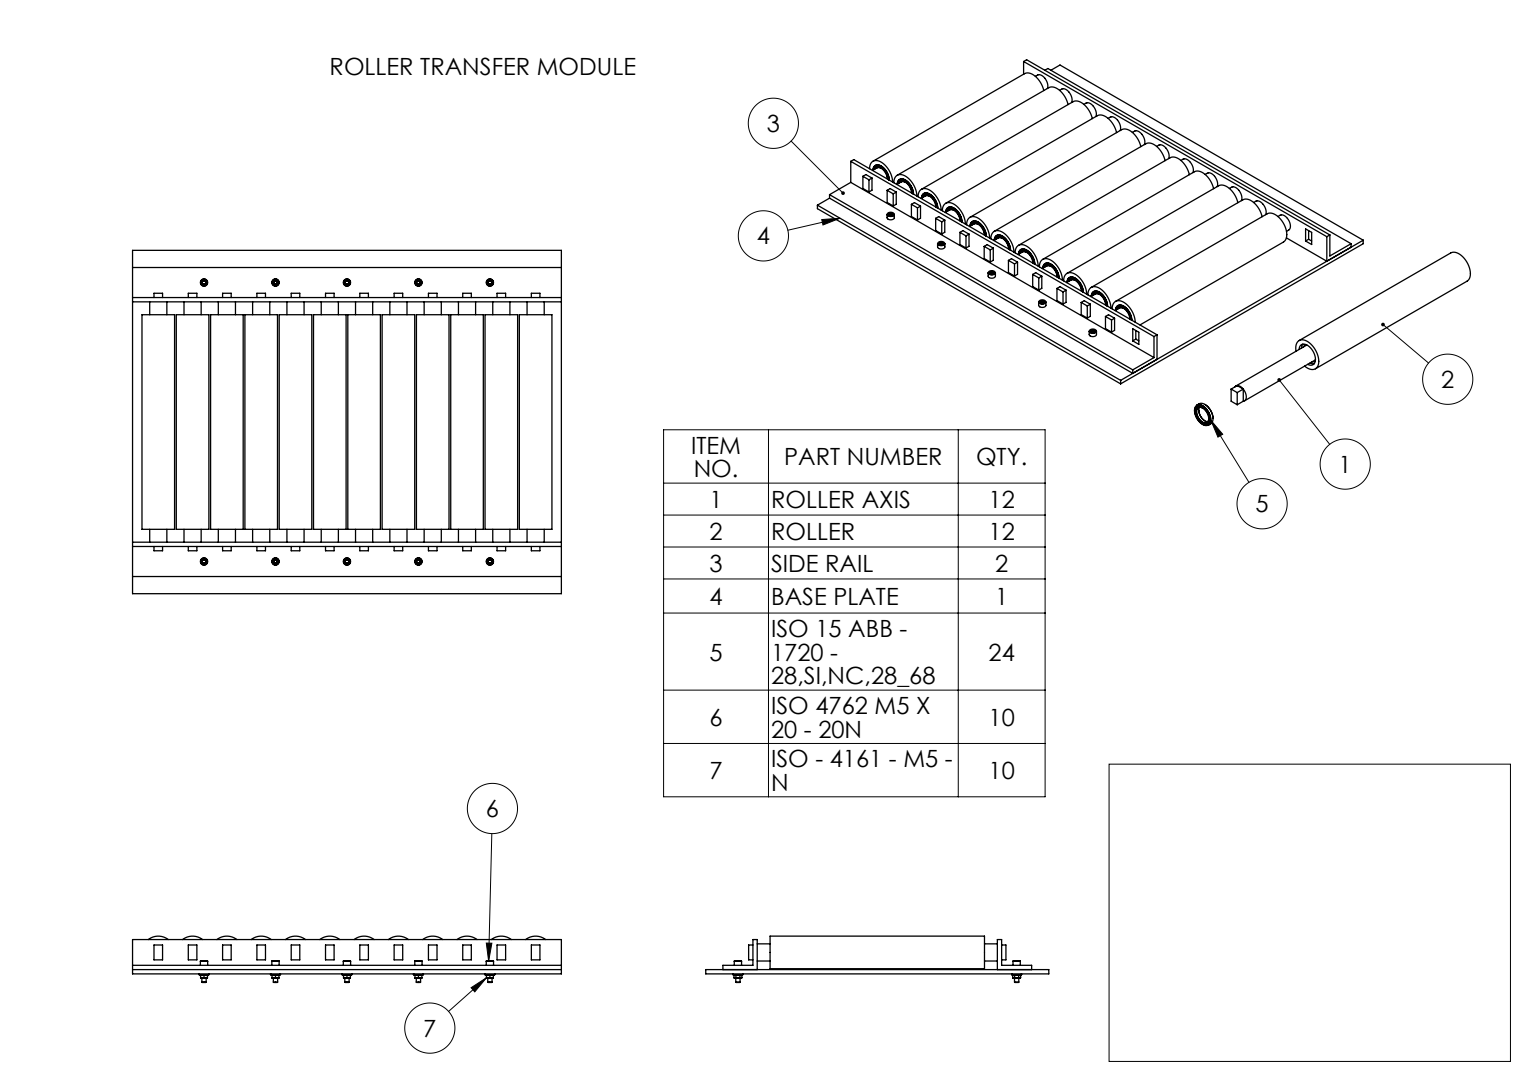
ISO-10303-21;
HEADER;
FILE_DESCRIPTION (('STEP AP214'),
    '1' );
FILE_NAME ('MAS-189',
    '2026-10-24T14:05:44',
    ( '' ),
    ( '' ),
    'SwSTEP 2.0',
    'SolidWorks 2026',
    '' );
FILE_SCHEMA (( 'AUTOMOTIVE_DESIGN' ));
ENDSEC;

DATA;
#1 = ORIENTED_EDGE ( 'NONE', *, *, #3686, .F. ) ;
#2 = ORIENTED_EDGE ( 'NONE', *, *, #1816, .F. ) ;
#3 = ORIENTED_EDGE ( 'NONE', *, *, #1318, .T. ) ;
#4 = CARTESIAN_POINT ( 'NONE',  ( 395.0000000000000000, -8.660254037844389075, 139.9990000000000236 ) ) ;
#5 = DIRECTION ( 'NONE',  ( -0.000000000000000000, -0.000000000000000000, 1.000000000000000000 ) ) ;
#6 = EDGE_CURVE ( 'NONE', #1873, #4758, #4106, .T. ) ;
#7 = VERTEX_POINT ( 'NONE', #676 ) ;
#8 = CARTESIAN_POINT ( 'NONE',  ( 53.33333333333330017, -20.00000000000000000, -165.1500000000000625 ) ) ;
#9 = CARTESIAN_POINT ( 'NONE',  ( 124.9999999999999858, 8.660254037844390851, 145.0000000000000284 ) ) ;
#10 = DIRECTION ( 'NONE',  ( 0.000000000000000000, 0.000000000000000000, 1.000000000000000000 ) ) ;
#11 = ORIENTED_EDGE ( 'NONE', *, *, #5026, .T. ) ;
#12 = PLANE ( 'NONE',  #5087 ) ;
#13 = EDGE_CURVE ( 'NONE', #2711, #3697, #5372, .T. ) ;
#14 = ORIENTED_EDGE ( 'NONE', *, *, #3601, .F. ) ;
#15 = DIRECTION ( 'NONE',  ( -0.000000000000000000, -0.000000000000000000, 1.000000000000000000 ) ) ;
#16 = CARTESIAN_POINT ( 'NONE',  ( 395.0000000000000000, 8.660254037844390851, 140.0000000000000000 ) ) ;
#17 = CONTEXT_DEPENDENT_SHAPE_REPRESENTATION ( #2675, #3582 ) ;
#18 = DIRECTION ( 'NONE',  ( -1.000000000000000000, 0.000000000000000000, 0.000000000000000000 ) ) ;
#19 = CARTESIAN_POINT ( 'NONE',  ( -4.000000000000000000, -2.309401076758512694, -5.000000000000000000 ) ) ;
#20 =( REPRESENTATION_RELATIONSHIP ('NONE','NONE', #5587, #1193 ) REPRESENTATION_RELATIONSHIP_WITH_TRANSFORMATION ( #1968 )SHAPE_REPRESENTATION_RELATIONSHIP( ) );
#21 = ORIENTED_EDGE ( 'NONE', *, *, #3815, .F. ) ;
#22 = CARTESIAN_POINT ( 'NONE',  ( 445.0000000000000000, 8.660254037844390851, 145.0000000000000284 ) ) ;
#23 = VECTOR ( 'NONE', #2608, 1000.000000000000000 ) ;
#24 = EDGE_CURVE ( 'NONE', #1078, #1538, #2930, .T. ) ;
#25 = ORIENTED_EDGE ( 'NONE', *, *, #1141, .F. ) ;
#26 = DIRECTION ( 'NONE',  ( 1.000000000000000000, 0.000000000000000000, 0.000000000000000000 ) ) ;
#27 = CARTESIAN_POINT ( 'NONE',  ( 0.000000000000000000, 0.000000000000000000, 140.0000000000000000 ) ) ;
#28 = CARTESIAN_POINT ( 'NONE',  ( 285.0000000000000568, 8.660254037844390851, 139.9990000000000236 ) ) ;
#29 = LINE ( 'NONE', #5746, #1486 ) ;
#30 = CIRCLE ( 'NONE', #5634, 2.041999999999999815 ) ;
#31 = COLOUR_RGB ( '',0.8941176470588234615, 0.8941176470588234615, 0.8941176470588234615 ) ;
#32 = CARTESIAN_POINT ( 'NONE',  ( 2.500000000000000000, 2.357898499370433054, -1.951563910473907981E-15 ) ) ;
#33 = AXIS2_PLACEMENT_3D ( 'NONE', #4684, #4191, #721 ) ;
#34 = ORIENTED_EDGE ( 'NONE', *, *, #6882, .F. ) ;
#35 = DIRECTION ( 'NONE',  ( 1.000000000000000000, 0.000000000000000000, 0.000000000000000000 ) ) ;
#36 = EDGE_LOOP ( 'NONE', ( #2850, #5154, #2627, #2005, #1100 ) ) ;
#37 = FILL_AREA_STYLE_COLOUR ( '', #3895 ) ;
#38 = AXIS2_PLACEMENT_3D ( 'NONE', #3689, #2086, #340 ) ;
#39 = DIRECTION ( 'NONE',  ( 0.000000000000000000, 0.000000000000000000, -1.000000000000000000 ) ) ;
#40 = ORIENTED_EDGE ( 'NONE', *, *, #976, .T. ) ;
#41 = AXIS2_PLACEMENT_3D ( 'NONE', #7313, #7278, #7239 ) ;
#42 = CARTESIAN_POINT ( 'NONE',  ( -4.000000000000000000, 2.309401076758498483, -0.4999999999999927280 ) ) ;
#43 = EDGE_CURVE ( 'NONE', #586, #2446, #6979, .T. ) ;
#44 = LINE ( 'NONE', #6748, #4124 ) ;
#45 = CARTESIAN_POINT ( 'NONE',  ( 219.9999999999999716, -10.00000000000000000, -162.5000000000000853 ) ) ;
#46 = ORIENTED_EDGE ( 'NONE', *, *, #4516, .T. ) ;
#47 = FACE_OUTER_BOUND ( 'NONE', #4847, .T. ) ;
#48 = ORIENTED_EDGE ( 'NONE', *, *, #1653, .T. ) ;
#49 = CARTESIAN_POINT ( 'NONE',  ( 0.000000000000000000, -15.00000000000000000, 145.0000000000000284 ) ) ;
#50 = CARTESIAN_POINT ( 'NONE',  ( 445.0000000000000000, 8.660254037844390851, 140.0000000000000000 ) ) ;
#51 = ITEM_DEFINED_TRANSFORMATION ( 'NONE', 'NONE', #3732,  #1963 ) ;
#52 = DIRECTION ( 'NONE',  ( 0.000000000000000000, -0.000000000000000000, 1.000000000000000000 ) ) ;
#53 = CARTESIAN_POINT ( 'NONE',  ( 4.999999999999997335, -8.660254037844389075, -140.0000000000000000 ) ) ;
#54 = EDGE_CURVE ( 'NONE', #6404, #2818, #2960, .T. ) ;
#55 = ORIENTED_EDGE ( 'NONE', *, *, #575, .F. ) ;
#56 = AXIS2_PLACEMENT_3D ( 'NONE', #6815, #5153, #4630 ) ;
#57 = FACE_OUTER_BOUND ( 'NONE', #1161, .T. ) ;
#58 = VECTOR ( 'NONE', #6647, 1000.000000000000000 ) ;
#59 = AXIS2_PLACEMENT_3D ( 'NONE', #3524, #1675, #1876 ) ;
#60 = EDGE_LOOP ( 'NONE', ( #5047, #1369, #5230, #2362 ) ) ;
#61 = APPLICATION_CONTEXT ( 'automotive_design' ) ;
#62 = FACE_OUTER_BOUND ( 'NONE', #5362, .T. ) ;
#63 = DIRECTION ( 'NONE',  ( 0.000000000000000000, -1.000000000000000000, 0.000000000000000000 ) ) ;
#64 = AXIS2_PLACEMENT_3D ( 'NONE', #2945, #3017, #209 ) ;
#65 = DIRECTION ( 'NONE',  ( 0.000000000000000000, 0.000000000000000000, 1.000000000000000000 ) ) ;
#66 = CARTESIAN_POINT ( 'NONE',  ( 2.500000000000000000, 0.000000000000000000, 2.041999999999999815 ) ) ;
#67 = EDGE_CURVE ( 'NONE', #3261, #4228, #2370, .T. ) ;
#68 = CARTESIAN_POINT ( 'NONE',  ( -4.000000000000000000, -2.309401076758512694, -3.433295621305382461 ) ) ;
#69 = AXIS2_PLACEMENT_3D ( 'NONE', #6445, #5876, #2455 ) ;
#70 = EDGE_CURVE ( 'NONE', #2423, #6108, #5233, .T. ) ;
#71 = ORIENTED_EDGE ( 'NONE', *, *, #6101, .T. ) ;
#72 = ORIENTED_EDGE ( 'NONE', *, *, #5764, .T. ) ;
#73 = AXIS2_PLACEMENT_3D ( 'NONE', #2890, #4175, #5910 ) ;
#74 = LINE ( 'NONE', #2335, #4027 ) ;
#75 = AXIS2_PLACEMENT_3D ( 'NONE', #5132, #5651, #4005 ) ;
#76 = VERTEX_POINT ( 'NONE', #5837 ) ;
#77 = AXIS2_PLACEMENT_3D ( 'NONE', #800, #3054, #1978 ) ;
#78 = ADVANCED_FACE ( 'NONE', ( #707 ), #151, .F. ) ;
#79 = CARTESIAN_POINT ( 'NONE',  ( 303.3333333333333144, -20.00000000000000000, 162.5000000000000853 ) ) ;
#80 = CARTESIAN_POINT ( 'NONE',  ( -5.000000000000000888, 8.660254037844390851, 150.0000000000000000 ) ) ;
#81 = ORIENTED_EDGE ( 'NONE', *, *, #6837, .T. ) ;
#82 = PRODUCT_DEFINITION_SHAPE ( 'NONE', 'NONE',  #7372 ) ;
#83 = DIRECTION ( 'NONE',  ( 1.000000000000000000, 0.000000000000000000, -0.000000000000000000 ) ) ;
#84 = VERTEX_POINT ( 'NONE', #1298 ) ;
#85 = EDGE_LOOP ( 'NONE', ( #6499, #7166 ) ) ;
#86 = DIRECTION ( 'NONE',  ( 0.000000000000000000, 0.8660254037844380415, -0.5000000000000011102 ) ) ;
#87 = AXIS2_PLACEMENT_3D ( 'NONE', #968, #3225, #5526 ) ;
#88 = DIRECTION ( 'NONE',  ( -0.000000000000000000, 1.000000000000000000, -0.000000000000000000 ) ) ;
#89 = CONTEXT_DEPENDENT_SHAPE_REPRESENTATION ( #5884, #565 ) ;
#90 = CARTESIAN_POINT ( 'NONE',  ( 435.0000000000000568, 8.660254037844390851, 140.0000000000000000 ) ) ;
#91 = CARTESIAN_POINT ( 'NONE',  ( -20.63749999999999929, 1.353234713057825478E-15, 11.05000000000000071 ) ) ;
#92 = ORIENTED_EDGE ( 'NONE', *, *, #7290, .F. ) ;
#93 = DIRECTION ( 'NONE',  ( 0.000000000000000000, 0.000000000000000000, 1.000000000000000000 ) ) ;
#94 = ADVANCED_FACE ( 'NONE', ( #3566 ), #5869, .F. ) ;
#95 = ORIENTED_EDGE ( 'NONE', *, *, #13, .T. ) ;
#96 = EDGE_CURVE ( 'NONE', #3309, #6744, #6473, .T. ) ;
#97 = DIRECTION ( 'NONE',  ( 1.000000000000000000, 0.000000000000000000, -0.000000000000000000 ) ) ;
#98 = AXIS2_PLACEMENT_3D ( 'NONE', #2545, #1752, #6896 ) ;
#99 = CARTESIAN_POINT ( 'NONE',  ( 155.0000000000000000, -8.660254037844389075, 139.9990000000000236 ) ) ;
#100 = LINE ( 'NONE', #5559, #7316 ) ;
#101 = CARTESIAN_POINT ( 'NONE',  ( 11.00000000000000000, 1.347111479062088405E-15, 121.0000000000000000 ) ) ;
#102 = ORIENTED_EDGE ( 'NONE', *, *, #2735, .T. ) ;
#103 = ORIENTED_EDGE ( 'NONE', *, *, #104, .F. ) ;
#104 = EDGE_CURVE ( 'NONE', #3497, #7, #5877, .T. ) ;
#105 = APPLICATION_PROTOCOL_DEFINITION ( 'draft international standard', 'automotive_design', 1998, #6326 ) ;
#106 = CARTESIAN_POINT ( 'NONE',  ( 155.0000000000000000, 8.660254037844390851, 140.0000000000000000 ) ) ;
#107 = EDGE_LOOP ( 'NONE', ( #5090, #2760, #2727, #2223 ) ) ;
#108 = DIRECTION ( 'NONE',  ( 1.000000000000000000, 0.000000000000000000, 0.000000000000000000 ) ) ;
#109 = PLANE ( 'NONE',  #1833 ) ;
#110 = DIRECTION ( 'NONE',  ( -0.000000000000000000, -0.000000000000000000, 1.000000000000000000 ) ) ;
#111 = ORIENTED_EDGE ( 'NONE', *, *, #1690, .F. ) ;
#112 =( REPRESENTATION_RELATIONSHIP ('NONE','NONE', #5587, #5023 ) REPRESENTATION_RELATIONSHIP_WITH_TRANSFORMATION ( #4149 )SHAPE_REPRESENTATION_RELATIONSHIP( ) );
#113 = EDGE_CURVE ( 'NONE', #3854, #1142, #3125, .T. ) ;
#114 = PRESENTATION_STYLE_ASSIGNMENT (( #5798 ) ) ;
#115 = DIRECTION ( 'NONE',  ( 0.000000000000000000, 0.000000000000000000, -1.000000000000000000 ) ) ;
#116 = CARTESIAN_POINT ( 'NONE',  ( 2.500000000000000000, 2.357898499370433054, -1.951563910473907981E-15 ) ) ;
#117 = PLANE ( 'NONE',  #3650 ) ;
#118 = ORIENTED_EDGE ( 'NONE', *, *, #6220, .F. ) ;
#119 = DIRECTION ( 'NONE',  ( 0.000000000000000000, 0.000000000000000000, 1.000000000000000000 ) ) ;
#120 = DIRECTION ( 'NONE',  ( 0.000000000000000000, 0.000000000000000000, -1.000000000000000000 ) ) ;
#121 = ITEM_DEFINED_TRANSFORMATION ( 'NONE', 'NONE', #6270,  #1963 ) ;
#122 = CARTESIAN_POINT ( 'NONE',  ( 0.6640947660595348800, -4.471078309994175548, -3.602146406945708090 ) ) ;
#123 = FACE_OUTER_BOUND ( 'NONE', #3816, .T. ) ;
#124 = ORIENTED_EDGE ( 'NONE', *, *, #2636, .T. ) ;
#125 = CARTESIAN_POINT ( 'NONE',  ( -6.473970235329672780E-16, -4.862606272033106691, -3.745885042887442395 ) ) ;
#126 = EDGE_LOOP ( 'NONE', ( #4642, #4899, #6680, #3898 ) ) ;
#127 = EDGE_LOOP ( 'NONE', ( #4208, #2738, #2635, #4055 ) ) ;
#128 = PLANE ( 'NONE',  #3351 ) ;
#129 = DIRECTION ( 'NONE',  ( 0.000000000000000000, 0.000000000000000000, 1.000000000000000000 ) ) ;
#130 = DIRECTION ( 'NONE',  ( 0.000000000000000000, 0.000000000000000000, 1.000000000000000000 ) ) ;
#131 = DIRECTION ( 'NONE',  ( 0.000000000000000000, -1.000000000000000000, 0.000000000000000000 ) ) ;
#132 = ADVANCED_FACE ( 'NONE', ( #414, #336 ), #6742, .T. ) ;
#133 = VECTOR ( 'NONE', #4306, 1000.000000000000000 ) ;
#134 = CARTESIAN_POINT ( 'NONE',  ( -3.349226789952655547, -2.685125164760744809, -0.2236248678334863682 ) ) ;
#135 = ORIENTED_EDGE ( 'NONE', *, *, #6168, .F. ) ;
#136 = EDGE_LOOP ( 'NONE', ( #7154, #5088, #1278, #4786 ) ) ;
#137 = CIRCLE ( 'NONE', #621, 1.050000000000000488 ) ;
#138 = ITEM_DEFINED_TRANSFORMATION ( 'NONE', 'NONE', #6293,  #1963 ) ;
#139 = DIRECTION ( 'NONE',  ( -0.000000000000000000, -1.000000000000000000, -0.000000000000000000 ) ) ;
#140 = EDGE_LOOP ( 'NONE', ( #451, #3034, #5054, #639, #3841, #3880, #6414, #6214 ) ) ;
#141 = SURFACE_STYLE_USAGE ( .BOTH. , #4095 ) ;
#142 = AXIS2_PLACEMENT_3D ( 'NONE', #4791, #2425, #751 ) ;
#143 = ADVANCED_FACE ( 'NONE', ( #298 ), #1009, .F. ) ;
#144 = CARTESIAN_POINT ( 'NONE',  ( -3.333333333333332149, -2.694301256218264218, -3.300726591567082036 ) ) ;
#145 = ADVANCED_FACE ( 'NONE', ( #6026 ), #5486, .F. ) ;
#146 =( BOUNDED_SURFACE ( )  B_SPLINE_SURFACE ( 3, 2, ( 
 ( #6466, #1910, #6397 ),
 ( #629, #5334, #5259 ),
 ( #1805, #4662, #5832 ),
 ( #1324, #4699, #1848 ),
 ( #734, #2886, #1879 ),
 ( #5298, #2440, #4772 ) ),
 .UNSPECIFIED., .F., .F., .F. ) 
 B_SPLINE_SURFACE_WITH_KNOTS ( ( 4, 2, 4 ),
 ( 3, 3 ),
 ( 0.02027752710269158445, 0.02273781595091097299, 0.02519810479913036153 ),
 ( 0.000000000000000000, 1.000000000000000000 ),
 .UNSPECIFIED. ) 
 GEOMETRIC_REPRESENTATION_ITEM ( )  RATIONAL_B_SPLINE_SURFACE ( (
 ( 1.000000000000000000, 0.8047781431712808242, 1.000000000000000000),
 ( 1.000000000000000000, 0.8123773247083928561, 1.000000000000000000),
 ( 1.000000000000000000, 0.8190670192154906326, 1.000000000000000000),
 ( 1.000000000000000000, 0.8192353552912178261, 1.000000000000000000),
 ( 1.000000000000000000, 0.8126132098226825917, 1.000000000000000000),
 ( 1.000000000000000000, 0.8047712465856394770, 1.000000000000000000) ) ) 
 REPRESENTATION_ITEM ( '' )  SURFACE ( )  );
#147 = EDGE_LOOP ( 'NONE', ( #2986, #2941 ) ) ;
#148 = CARTESIAN_POINT ( 'NONE',  ( 4.000000000000000000, 2.309401076758497151, -5.000000000000000000 ) ) ;
#149 = CARTESIAN_POINT ( 'NONE',  ( -5.000000000000000888, -8.660254037844389075, -150.0000000000000000 ) ) ;
#150 = EDGE_CURVE ( 'NONE', #1987, #1784, #6703, .T. ) ;
#151 = CYLINDRICAL_SURFACE ( 'NONE', #6391, 13.50000000000000000 ) ;
#152 = DIRECTION ( 'NONE',  ( -0.000000000000000000, 1.000000000000000000, 0.000000000000000000 ) ) ;
#153 = VERTEX_POINT ( 'NONE', #2555 ) ;
#154 = TOROIDAL_SURFACE ( 'NONE', #6366, 10.20000000000000107, 0.2000000000000031197 ) ;
#155 = VECTOR ( 'NONE', #4751, 1000.000000000000000 ) ;
#156 = CARTESIAN_POINT ( 'NONE',  ( 2.500000000000000000, -1.178949249685213863, 2.042000000000002924 ) ) ;
#157 = DIRECTION ( 'NONE',  ( 0.000000000000000000, 1.000000000000000000, 0.000000000000000000 ) ) ;
#158 = CONTEXT_DEPENDENT_SHAPE_REPRESENTATION ( #3529, #1322 ) ;
#159 = CARTESIAN_POINT ( 'NONE',  ( -1.999999999999998224, 1.353234713057825478E-15, 11.05000000000000071 ) ) ;
#160 = DIRECTION ( 'NONE',  ( 0.000000000000000000, 0.000000000000000000, 1.000000000000000000 ) ) ;
#161 = ORIENTED_EDGE ( 'NONE', *, *, #6818, .T. ) ;
#162 = CARTESIAN_POINT ( 'NONE',  ( 0.000000000000000000, 0.000000000000000000, -5.000000000000000000 ) ) ;
#163 = ORIENTED_EDGE ( 'NONE', *, *, #1002, .T. ) ;
#164 = ORIENTED_EDGE ( 'NONE', *, *, #4721, .T. ) ;
#165 = CARTESIAN_POINT ( 'NONE',  ( 84.99999999999998579, 8.660254037844390851, 145.0000000000000284 ) ) ;
#166 = CARTESIAN_POINT ( 'NONE',  ( -3.455068668934486276, 2.624017327439035707, -3.316620875263955437 ) ) ;
#167 = PLANE ( 'NONE',  #1333 ) ;
#168 = CARTESIAN_POINT ( 'NONE',  ( -0.3208286057739654917, 4.433571671609680465, -0.3503314178412548774 ) ) ;
#169 =( GEOMETRIC_REPRESENTATION_CONTEXT ( 3 ) GLOBAL_UNCERTAINTY_ASSIGNED_CONTEXT ( ( #1828 ) ) GLOBAL_UNIT_ASSIGNED_CONTEXT ( ( #2358, #5677, #5718 ) ) REPRESENTATION_CONTEXT ( 'NONE', 'WORKASPACE' ) );
#170 =( GEOMETRIC_REPRESENTATION_CONTEXT ( 3 ) GLOBAL_UNCERTAINTY_ASSIGNED_CONTEXT ( ( #6164 ) ) GLOBAL_UNIT_ASSIGNED_CONTEXT ( ( #1926, #3047, #2969 ) ) REPRESENTATION_CONTEXT ( 'NONE', 'WORKASPACE' ) );
#171 = AXIS2_PLACEMENT_3D ( 'NONE', #6654, #216, #2471 ) ;
#172 = DIRECTION ( 'NONE',  ( -1.000000000000000000, 0.000000000000000000, 0.000000000000000000 ) ) ;
#173 = AXIS2_PLACEMENT_3D ( 'NONE', #885, #1525, #6178 ) ;
#174 = ORIENTED_EDGE ( 'NONE', *, *, #1060, .T. ) ;
#175 = EDGE_CURVE ( 'NONE', #2749, #3012, #3113, .T. ) ;
#176 = VECTOR ( 'NONE', #5935, 1000.000000000000000 ) ;
#177 = CIRCLE ( 'NONE', #883, 12.77500000000000036 ) ;
#178 = DIRECTION ( 'NONE',  ( 0.000000000000000000, 0.000000000000000000, 1.000000000000000000 ) ) ;
#179 = ORIENTED_EDGE ( 'NONE', *, *, #5269, .F. ) ;
#180 = VECTOR ( 'NONE', #724, 1000.000000000000114 ) ;
#181 = CIRCLE ( 'NONE', #4359, 10.00000000000000000 ) ;
#182 = CARTESIAN_POINT ( 'NONE',  ( -2.000000000000002665, -3.464101615137770374, -3.142992957459237680 ) ) ;
#183 = VERTEX_POINT ( 'NONE', #4979 ) ;
#184 = EDGE_CURVE ( 'NONE', #3899, #7, #6874, .T. ) ;
#185 = CIRCLE ( 'NONE', #4719, 0.2500000000000002220 ) ;
#186 = AXIS2_PLACEMENT_3D ( 'NONE', #6710, #5457, #2041 ) ;
#187 = ADVANCED_FACE ( 'NONE', ( #3805 ), #4852, .F. ) ;
#188 = DIRECTION ( 'NONE',  ( 0.000000000000000000, 0.000000000000000000, 1.000000000000000000 ) ) ;
#189 = CARTESIAN_POINT ( 'NONE',  ( 4.999999999999999112, 8.660254037844390851, 150.0000000000000000 ) ) ;
#190 = VECTOR ( 'NONE', #1081, 1000.000000000000000 ) ;
#191 = FACE_OUTER_BOUND ( 'NONE', #1286, .T. ) ;
#192 = ORIENTED_EDGE ( 'NONE', *, *, #3648, .F. ) ;
#193 = EDGE_CURVE ( 'NONE', #2007, #224, #1714, .T. ) ;
#194 = CARTESIAN_POINT ( 'NONE',  ( 114.9999999999999858, -8.660254037844389075, 145.0000000000000284 ) ) ;
#195 = ITEM_DEFINED_TRANSFORMATION ( 'NONE', 'NONE', #6279,  #1963 ) ;
#196 = FACE_OUTER_BOUND ( 'NONE', #2058, .T. ) ;
#197 = CARTESIAN_POINT ( 'NONE',  ( 470.0000000000000000, 0.000000000000000000, 140.0000000000000000 ) ) ;
#198 = DIRECTION ( 'NONE',  ( 0.000000000000000000, 0.000000000000000000, 1.000000000000000000 ) ) ;
#199 = ORIENTED_EDGE ( 'NONE', *, *, #1070, .F. ) ;
#200 = DIRECTION ( 'NONE',  ( 1.000000000000000000, 0.000000000000000000, 0.000000000000000000 ) ) ;
#201 = ORIENTED_EDGE ( 'NONE', *, *, #1503, .T. ) ;
#202 = CIRCLE ( 'NONE', #2702, 2.499999999999999556 ) ;
#203 = PRODUCT_DEFINITION_SHAPE ( 'NONE', 'NONE',  #7381 ) ;
#204 = ORIENTED_EDGE ( 'NONE', *, *, #2954, .T. ) ;
#205 = ADVANCED_FACE ( 'NONE', ( #4414 ), #1489, .F. ) ;
#206 = LINE ( 'NONE', #6379, #2632 ) ;
#207 = CARTESIAN_POINT ( 'NONE',  ( -0.5449313310646672903, -4.304185902836978883, -3.316620875263469159 ) ) ;
#208 = CARTESIAN_POINT ( 'NONE',  ( -4.000000000000000000, 0.000000000000000000, 0.000000000000000000 ) ) ;
#209 = DIRECTION ( 'NONE',  ( 0.000000000000000000, 0.000000000000000000, 1.000000000000000000 ) ) ;
#210 = VECTOR ( 'NONE', #6991, 1000.000000000000000 ) ;
#211 = CARTESIAN_POINT ( 'NONE',  ( 205.0000000000000284, -8.660254037844389075, 139.9990000000000236 ) ) ;
#212 = LINE ( 'NONE', #4197, #176 ) ;
#213 = PRODUCT_DEFINITION ( 'UNKNOWN', '', #6388, #5035 ) ;
#214 = VERTEX_POINT ( 'NONE', #7299 ) ;
#215 = CONTEXT_DEPENDENT_SHAPE_REPRESENTATION ( #1020, #5961 ) ;
#216 = DIRECTION ( 'NONE',  ( 1.000000000000000000, 0.000000000000000000, 0.000000000000000000 ) ) ;
#217 = ORIENTED_EDGE ( 'NONE', *, *, #4171, .T. ) ;
#218 = LINE ( 'NONE', #669, #6668 ) ;
#219 = ORIENTED_EDGE ( 'NONE', *, *, #5940, .T. ) ;
#220 = ORIENTED_EDGE ( 'NONE', *, *, #7013, .F. ) ;
#221 = DIRECTION ( 'NONE',  ( 0.000000000000000000, -1.000000000000000000, 0.000000000000000000 ) ) ;
#222 = DIRECTION ( 'NONE',  ( 1.000000000000000000, 0.000000000000000000, 0.000000000000000000 ) ) ;
#223 = ADVANCED_FACE ( 'NONE', ( #7142 ), #1996, .F. ) ;
#224 = VERTEX_POINT ( 'NONE', #6579 ) ;
#225 = CARTESIAN_POINT ( 'NONE',  ( 136.6666666666666288, -15.00000000000000000, 162.5000000000000853 ) ) ;
#226 = ORIENTED_EDGE ( 'NONE', *, *, #2907, .F. ) ;
#227 = DIRECTION ( 'NONE',  ( 0.000000000000000000, -0.000000000000000000, 1.000000000000000000 ) ) ;
#228 = CONTEXT_DEPENDENT_SHAPE_REPRESENTATION ( #5222, #7070 ) ;
#229 = CARTESIAN_POINT ( 'NONE',  ( 75.00000000000001421, -8.660254037844389075, 145.0000000000000284 ) ) ;
#230 = CARTESIAN_POINT ( 'NONE',  ( 24.55500000000002103, 0.000000000000000000, 0.000000000000000000 ) ) ;
#231 = DIRECTION ( 'NONE',  ( 1.000000000000000000, 0.000000000000000000, 0.000000000000000000 ) ) ;
#232 = EDGE_LOOP ( 'NONE', ( #859, #5751, #5107, #3402 ) ) ;
#233 = CARTESIAN_POINT ( 'NONE',  ( -1.800000000000002931, 0.000000000000000000, -13.50000000000000355 ) ) ;
#234 = EDGE_CURVE ( 'NONE', #6037, #2259, #3253, .T. ) ;
#235 = EDGE_CURVE ( 'NONE', #4841, #4123, #4707, .T. ) ;
#236 = ORIENTED_EDGE ( 'NONE', *, *, #593, .T. ) ;
#237 = ORIENTED_EDGE ( 'NONE', *, *, #4529, .F. ) ;
#238 = DIRECTION ( 'NONE',  ( 1.000000000000000000, 0.000000000000000000, 0.000000000000000000 ) ) ;
#239 = CARTESIAN_POINT ( 'NONE',  ( 285.0000000000000568, -8.660254037844389075, 140.0000000000000000 ) ) ;
#240 = LINE ( 'NONE', #1936, #5296 ) ;
#241 = CARTESIAN_POINT ( 'NONE',  ( 0.000000000000000000, 15.00000000000000000, 145.0000000000000284 ) ) ;
#242 = CARTESIAN_POINT ( 'NONE',  ( -0.7826237921249277196, 0.000000000000000000, -11.05000000000000071 ) ) ;
#243 = DIRECTION ( 'NONE',  ( -0.000000000000000000, -1.000000000000000000, -0.000000000000000000 ) ) ;
#244 = ADVANCED_FACE ( 'NONE', ( #3311 ), #5610, .F. ) ;
#245 = EDGE_LOOP ( 'NONE', ( #1865, #2331, #5916, #510 ) ) ;
#246 = LINE ( 'NONE', #1986, #5667 ) ;
#247 = EDGE_LOOP ( 'NONE', ( #1984, #1651 ) ) ;
#248 = AXIS2_PLACEMENT_3D ( 'NONE', #5345, #1301, #1857 ) ;
#249 =( REPRESENTATION_RELATIONSHIP ('NONE','NONE', #5587, #1193 ) REPRESENTATION_RELATIONSHIP_WITH_TRANSFORMATION ( #3241 )SHAPE_REPRESENTATION_RELATIONSHIP( ) );
#250 = DIRECTION ( 'NONE',  ( -0.000000000000000000, -0.000000000000000000, 1.000000000000000000 ) ) ;
#251 = EDGE_LOOP ( 'NONE', ( #4553, #3750, #2974 ) ) ;
#252 = ORIENTED_EDGE ( 'NONE', *, *, #6107, .T. ) ;
#253 = DIRECTION ( 'NONE',  ( 1.000000000000000000, 0.000000000000000000, 0.000000000000000000 ) ) ;
#254 = AXIS2_PLACEMENT_3D ( 'NONE', #4363, #7167, #6172 ) ;
#255 = CARTESIAN_POINT ( 'NONE',  ( 5.000000000000002665, 3.306546357697854226E-16, 2.700000000000001066 ) ) ;
#256 = AXIS2_PLACEMENT_3D ( 'NONE', #4917, #1432, #2617 ) ;
#257 = CARTESIAN_POINT ( 'NONE',  ( 315.0000000000000568, -8.660254037844389075, 140.0000000000000000 ) ) ;
#258 = DIRECTION ( 'NONE',  ( 0.000000000000000000, 0.000000000000000000, 1.000000000000000000 ) ) ;
#259 = ORIENTED_EDGE ( 'NONE', *, *, #7249, .T. ) ;
#260 = EDGE_CURVE ( 'NONE', #6697, #3198, #4705, .T. ) ;
#261 = CARTESIAN_POINT ( 'NONE',  ( 155.0000000000000000, -8.660254037844389075, 140.0000000000000000 ) ) ;
#262 = CONTEXT_DEPENDENT_SHAPE_REPRESENTATION ( #7035, #3652 ) ;
#263 = FACE_OUTER_BOUND ( 'NONE', #980, .T. ) ;
#264 = FACE_BOUND ( 'NONE', #5011, .T. ) ;
#265 =( NAMED_UNIT ( * ) SI_UNIT ( $, .STERADIAN. ) SOLID_ANGLE_UNIT ( ) );
#266 = VERTEX_POINT ( 'NONE', #5591 ) ;
#267 = CARTESIAN_POINT ( 'NONE',  ( -30.00000000000002842, -25.00000000000000000, 200.0000000000000000 ) ) ;
#268 = VECTOR ( 'NONE', #2901, 1000.000000000000000 ) ;
#269 = CIRCLE ( 'NONE', #2514, 2.700000000000001066 ) ;
#270 = EDGE_LOOP ( 'NONE', ( #4562, #2642, #3937, #2477 ) ) ;
#271 = VERTEX_POINT ( 'NONE', #4467 ) ;
#272 = CARTESIAN_POINT ( 'NONE',  ( -30.00000000000000000, 0.000000000000000000, 145.0000000000000284 ) ) ;
#273 = CARTESIAN_POINT ( 'NONE',  ( -4.235886605889389145, -2.417314728048544303, -3.751161874094020909 ) ) ;
#274 = LINE ( 'NONE', #4831, #5071 ) ;
#275 = LINE ( 'NONE', #241, #3751 ) ;
#276 = ADVANCED_FACE ( 'NONE', ( #508 ), #4512, .F. ) ;
#277 = VECTOR ( 'NONE', #2807, 1000.000000000000000 ) ;
#278 = DIRECTION ( 'NONE',  ( 0.000000000000000000, 1.000000000000000000, -1.224646799147353207E-16 ) ) ;
#279 = FACE_OUTER_BOUND ( 'NONE', #3322, .T. ) ;
#280 = ORIENTED_EDGE ( 'NONE', *, *, #5520, .F. ) ;
#281 = PRODUCT_DEFINITION_SHAPE ( 'NONE', 'NONE',  #7360 ) ;
#282 = ITEM_DEFINED_TRANSFORMATION ( 'NONE', 'NONE', #2061,  #1963 ) ;
#283 = CARTESIAN_POINT ( 'NONE',  ( 219.9999999999999716, -25.00000000000000000, -165.1500000000000625 ) ) ;
#284 = ORIENTED_EDGE ( 'NONE', *, *, #5933, .F. ) ;
#285 = CARTESIAN_POINT ( 'NONE',  ( 303.3333333333333144, -25.00000000000000000, -162.5000000000000853 ) ) ;
#286 = EDGE_CURVE ( 'NONE', #7309, #3129, #6272, .T. ) ;
#287 =( NAMED_UNIT ( * ) SI_UNIT ( $, .STERADIAN. ) SOLID_ANGLE_UNIT ( ) );
#288 = EDGE_CURVE ( 'NONE', #5585, #1382, #4104, .T. ) ;
#289 = FACE_OUTER_BOUND ( 'NONE', #1974, .T. ) ;
#290 = DIRECTION ( 'NONE',  ( 0.000000000000000000, 1.000000000000000000, -1.471414886128461471E-15 ) ) ;
#291 = VECTOR ( 'NONE', #1291, 1000.000000000000000 ) ;
#292 = ORIENTED_EDGE ( 'NONE', *, *, #3168, .F. ) ;
#293 = ORIENTED_EDGE ( 'NONE', *, *, #6948, .T. ) ;
#294 =( REPRESENTATION_RELATIONSHIP ('NONE','NONE', #5587, #6025 ) REPRESENTATION_RELATIONSHIP_WITH_TRANSFORMATION ( #5363 )SHAPE_REPRESENTATION_RELATIONSHIP( ) );
#295 = DIRECTION ( 'NONE',  ( 0.000000000000000000, 1.000000000000000000, 0.000000000000000000 ) ) ;
#296 = AXIS2_PLACEMENT_3D ( 'NONE', #6685, #4909, #7197 ) ;
#297 = CARTESIAN_POINT ( 'NONE',  ( -5.384454397937118664, 6.594054843588581554E-16, -4.484454397937119197 ) ) ;
#298 = FACE_OUTER_BOUND ( 'NONE', #2619, .T. ) ;
#299 = CARTESIAN_POINT ( 'NONE',  ( 0.000000000000000000, 0.000000000000000000, 125.0000000000000000 ) ) ;
#300 = ORIENTED_EDGE ( 'NONE', *, *, #2593, .F. ) ;
#301 = ADVANCED_FACE ( 'NONE', ( #5506 ), #2054, .T. ) ;
#302 = LINE ( 'NONE', #894, #3741 ) ;
#303 = CYLINDRICAL_SURFACE ( 'NONE', #4799, 2.649999999999985700 ) ;
#304 = CARTESIAN_POINT ( 'NONE',  ( 35.00000000000000000, -8.660254037844389075, 145.0000000000000284 ) ) ;
#305 = VECTOR ( 'NONE', #531, 1000.000000000000000 ) ;
#306 = CARTESIAN_POINT ( 'NONE',  ( 386.6666666666666288, -10.00000000000000000, 162.5000000000000853 ) ) ;
#307 = EDGE_LOOP ( 'NONE', ( #1128, #3991, #4538, #5321 ) ) ;
#308 = DIRECTION ( 'NONE',  ( -0.000000000000000000, 0.000000000000000000, -1.000000000000000000 ) ) ;
#309 = ORIENTED_EDGE ( 'NONE', *, *, #948, .F. ) ;
#310 = VERTEX_POINT ( 'NONE', #3745 ) ;
#311 = CIRCLE ( 'NONE', #2556, 12.77500000000000036 ) ;
#312 = ORIENTED_EDGE ( 'NONE', *, *, #4187, .T. ) ;
#313 = DIRECTION ( 'NONE',  ( 0.000000000000000000, 0.000000000000000000, 1.000000000000000000 ) ) ;
#314 = AXIS2_PLACEMENT_3D ( 'NONE', #1589, #3208, #5511 ) ;
#315 = LINE ( 'NONE', #4230, #906 ) ;
#316 = CARTESIAN_POINT ( 'NONE',  ( 0.2500000000000002220, 0.000000000000000000, 4.000000000000000000 ) ) ;
#317 = CARTESIAN_POINT ( 'NONE',  ( 386.6666666666666288, -20.00000000000000000, 165.1500000000000625 ) ) ;
#318 = CARTESIAN_POINT ( 'NONE',  ( 5.200000000000002842, 3.306546357697854719E-16, 2.700000000000001066 ) ) ;
#319 = EDGE_CURVE ( 'NONE', #5864, #3377, #5467, .T. ) ;
#320 = CARTESIAN_POINT ( 'NONE',  ( -2.000000000000001776, 1.641026710857453312E-15, 13.29999999999999893 ) ) ;
#321 = AXIS2_PLACEMENT_3D ( 'NONE', #471, #4507, #6798 ) ;
#322 = ORIENTED_EDGE ( 'NONE', *, *, #1493, .T. ) ;
#323 = PLANE ( 'NONE',  #7068 ) ;
#324 = DIRECTION ( 'NONE',  ( 0.000000000000000000, 0.000000000000000000, -1.000000000000000000 ) ) ;
#325 = ORIENTED_EDGE ( 'NONE', *, *, #3553, .T. ) ;
#326 = FACE_OUTER_BOUND ( 'NONE', #3436, .T. ) ;
#327 = DIRECTION ( 'NONE',  ( 0.000000000000000000, -0.000000000000000000, 1.000000000000000000 ) ) ;
#328 = DIRECTION ( 'NONE',  ( 1.000000000000000000, 0.000000000000000000, 0.000000000000000000 ) ) ;
#329 = EDGE_CURVE ( 'NONE', #5766, #3104, #1067, .T. ) ;
#330 = ORIENTED_EDGE ( 'NONE', *, *, #694, .F. ) ;
#331 = ADVANCED_FACE ( 'NONE', ( #6163 ), #6723, .T. ) ;
#332 = DIRECTION ( 'NONE',  ( 1.000000000000000000, 0.000000000000000000, 0.000000000000000000 ) ) ;
#333 = EDGE_LOOP ( 'NONE', ( #4442, #2385, #6375, #2319 ) ) ;
#334 =( GEOMETRIC_REPRESENTATION_CONTEXT ( 3 ) GLOBAL_UNCERTAINTY_ASSIGNED_CONTEXT ( ( #6417 ) ) GLOBAL_UNIT_ASSIGNED_CONTEXT ( ( #4283, #1950, #1436 ) ) REPRESENTATION_CONTEXT ( 'NONE', 'WORKASPACE' ) );
#335 = CARTESIAN_POINT ( 'NONE',  ( 35.00000000000000000, 8.660254037844390851, 140.0000000000000000 ) ) ;
#336 = FACE_OUTER_BOUND ( 'NONE', #85, .T. ) ;
#337 = EDGE_CURVE ( 'NONE', #6618, #3696, #5673, .T. ) ;
#338 = ORIENTED_EDGE ( 'NONE', *, *, #2679, .T. ) ;
#339 = CARTESIAN_POINT ( 'NONE',  ( 4.000000000000000000, -0.8732470631449981147, -3.223155494240760088 ) ) ;
#340 = DIRECTION ( 'NONE',  ( 0.000000000000000000, -0.000000000000000000, -1.000000000000000000 ) ) ;
#341 = DIRECTION ( 'NONE',  ( -1.000000000000000000, 0.000000000000000000, 0.000000000000000000 ) ) ;
#342 = DIRECTION ( 'NONE',  ( 1.000000000000000000, 6.123233995736766036E-17, -6.123233995736764803E-17 ) ) ;
#343 = ORIENTED_EDGE ( 'NONE', *, *, #1444, .F. ) ;
#344 = CARTESIAN_POINT ( 'NONE',  ( 136.6666666666666288, -20.00000000000000000, 165.1500000000000625 ) ) ;
#345 = PRODUCT_DEFINITION_SHAPE ( 'NONE', 'NONE',  #6385 ) ;
#346 = CYLINDRICAL_SURFACE ( 'NONE', #6243, 2.649999999999985700 ) ;
#347 = EDGE_LOOP ( 'NONE', ( #5848, #2567, #5256, #892 ) ) ;
#348 = EDGE_LOOP ( 'NONE', ( #1624, #5425 ) ) ;
#349 =( REPRESENTATION_RELATIONSHIP ('NONE','NONE', #5587, #5294 ) REPRESENTATION_RELATIONSHIP_WITH_TRANSFORMATION ( #5874 )SHAPE_REPRESENTATION_RELATIONSHIP( ) );
#350 = DIRECTION ( 'NONE',  ( -1.000000000000000000, -0.000000000000000000, -0.000000000000000000 ) ) ;
#351 = CARTESIAN_POINT ( 'NONE',  ( 4.000000000000000888, 1.563622288139206118, -0.2253451193528334950 ) ) ;
#352 = CYLINDRICAL_SURFACE ( 'NONE', #41, 10.00000000000000000 ) ;
#353 = CARTESIAN_POINT ( 'NONE',  ( -20.63749999999999929, 0.000000000000000000, 0.000000000000000000 ) ) ;
#354 = DIRECTION ( 'NONE',  ( 0.000000000000000000, 0.000000000000000000, -1.000000000000000000 ) ) ;
#355 = DIRECTION ( 'NONE',  ( 0.000000000000000000, 0.4999999999999993339, -0.8660254037844390407 ) ) ;
#356 = CARTESIAN_POINT ( 'NONE',  ( -6.259644161404862988E-16, -4.618802153517027165, -3.504271511726793076 ) ) ;
#357 = ORIENTED_EDGE ( 'NONE', *, *, #1783, .F. ) ;
#358 = LINE ( 'NONE', #4400, #970 ) ;
#359 = DIRECTION ( 'NONE',  ( -0.000000000000000000, -0.000000000000000000, -1.000000000000000000 ) ) ;
#360 = ORIENTED_EDGE ( 'NONE', *, *, #1641, .T. ) ;
#361 = EDGE_CURVE ( 'NONE', #380, #4483, #3166, .T. ) ;
#362 = DIRECTION ( 'NONE',  ( -1.000000000000000000, 0.000000000000000000, 0.000000000000000000 ) ) ;
#363 = FACE_OUTER_BOUND ( 'NONE', #5495, .T. ) ;
#364 = ORIENTED_EDGE ( 'NONE', *, *, #2779, .F. ) ;
#365 = DIRECTION ( 'NONE',  ( -1.000000000000000000, -6.123233995736766036E-17, -6.123233995736764803E-17 ) ) ;
#366 = ORIENTED_EDGE ( 'NONE', *, *, #235, .T. ) ;
#367 = CARTESIAN_POINT ( 'NONE',  ( 355.0000000000000000, -8.660254037844389075, 145.0000000000000284 ) ) ;
#368 = EDGE_CURVE ( 'NONE', #3826, #310, #7198, .T. ) ;
#369 = AXIS2_PLACEMENT_3D ( 'NONE', #1171, #3902, #2166 ) ;
#370 = ADVANCED_FACE ( 'NONE', ( #475 ), #3330, .F. ) ;
#371 = DIRECTION ( 'NONE',  ( -0.000000000000000000, 0.000000000000000000, 1.000000000000000000 ) ) ;
#372 = EDGE_LOOP ( 'NONE', ( #4500, #2241, #5481, #4153 ) ) ;
#373 = VECTOR ( 'NONE', #1246, 1000.000000000000000 ) ;
#374 = MECHANICAL_DESIGN_GEOMETRIC_PRESENTATION_REPRESENTATION (  '', ( #6844 ), #3015 ) ;
#375 = CARTESIAN_POINT ( 'NONE',  ( 4.211399257449709665, -2.459727064652517114, -3.751161691472417736 ) ) ;
#376 = DIRECTION ( 'NONE',  ( 1.000000000000000000, 0.000000000000000000, 0.000000000000000000 ) ) ;
#377 = FACE_BOUND ( 'NONE', #5167, .T. ) ;
#378 = ADVANCED_FACE ( 'NONE', ( #2736 ), #2063, .T. ) ;
#379 = CARTESIAN_POINT ( 'NONE',  ( 80.00000000000000000, 0.000000000000000000, 0.000000000000000000 ) ) ;
#380 = VERTEX_POINT ( 'NONE', #949 ) ;
#381 = FACE_OUTER_BOUND ( 'NONE', #2480, .T. ) ;
#382 = AXIS2_PLACEMENT_3D ( 'NONE', #5714, #6317, #1103 ) ;
#383 = EDGE_LOOP ( 'NONE', ( #6223, #1224 ) ) ;
#384 = ORIENTED_EDGE ( 'NONE', *, *, #3152, .F. ) ;
#385 = DIRECTION ( 'NONE',  ( -0.000000000000000000, -0.000000000000000000, 1.000000000000000000 ) ) ;
#386 = CARTESIAN_POINT ( 'NONE',  ( 4.235886605889389145, 2.417314728048528760, -3.751161874094018245 ) ) ;
#387 = CONTEXT_DEPENDENT_SHAPE_REPRESENTATION ( #1162, #1809 ) ;
#388 = CARTESIAN_POINT ( 'NONE',  ( 315.0000000000000568, -8.660254037844389075, 145.0000000000000284 ) ) ;
#389 = DIRECTION ( 'NONE',  ( 0.000000000000000000, 1.000000000000000000, -1.471414886128461471E-15 ) ) ;
#390 = TOROIDAL_SURFACE ( 'NONE', #1109, 11.75000000000000000, 1.050000000000000266 ) ;
#391 = CARTESIAN_POINT ( 'NONE',  ( -30.00000000000002842, -25.00000000000000000, 200.0000000000000000 ) ) ;
#392 = FACE_OUTER_BOUND ( 'NONE', #2164, .T. ) ;
#393 =( REPRESENTATION_RELATIONSHIP ('NONE','NONE', #5587, #5023 ) REPRESENTATION_RELATIONSHIP_WITH_TRANSFORMATION ( #6460 )SHAPE_REPRESENTATION_RELATIONSHIP( ) );
#394 = ORIENTED_EDGE ( 'NONE', *, *, #4580, .T. ) ;
#395 = EDGE_CURVE ( 'NONE', #3857, #5898, #757, .T. ) ;
#396 = CIRCLE ( 'NONE', #2290, 0.5155456020628804703 ) ;
#397 = FACE_OUTER_BOUND ( 'NONE', #140, .T. ) ;
#398 = LINE ( 'NONE', #994, #4132 ) ;
#399 = CARTESIAN_POINT ( 'NONE',  ( 0.000000000000000000, 0.000000000000000000, 0.000000000000000000 ) ) ;
#400 = FILL_AREA_STYLE ('',( #3302 ) ) ;
#401 = LINE ( 'NONE', #3139, #1706 ) ;
#402 = ADVANCED_BREP_SHAPE_REPRESENTATION ( '', ( #3126, #1963 ), #3131 ) ;
#403 = DIRECTION ( 'NONE',  ( -0.000000000000000000, -1.000000000000000000, -0.000000000000000000 ) ) ;
#404 = ORIENTED_EDGE ( 'NONE', *, *, #43, .T. ) ;
#405 = AXIS2_PLACEMENT_3D ( 'NONE', #1576, #6078, #4992 ) ;
#406 = EDGE_LOOP ( 'NONE', ( #4251, #4299, #5740, #309 ) ) ;
#407 = DIRECTION ( 'NONE',  ( 0.000000000000000000, 0.000000000000000000, 1.000000000000000000 ) ) ;
#408 = ORIENTED_EDGE ( 'NONE', *, *, #941, .F. ) ;
#409 = CARTESIAN_POINT ( 'NONE',  ( 4.999999999999999112, -8.660254037844389075, 140.0000000000000000 ) ) ;
#410 = CIRCLE ( 'NONE', #1470, 4.000000000000000000 ) ;
#411 = AXIS2_PLACEMENT_3D ( 'NONE', #3763, #2117, #332 ) ;
#412 = AXIS2_PLACEMENT_3D ( 'NONE', #4911, #6123, #5072 ) ;
#413 = CIRCLE ( 'NONE', #4342, 0.2000000000000000944 ) ;
#414 = FACE_BOUND ( 'NONE', #6136, .T. ) ;
#415 = CARTESIAN_POINT ( 'NONE',  ( -20.63749999999999574, 0.000000000000000000, 0.000000000000000000 ) ) ;
#416 = EDGE_CURVE ( 'NONE', #2352, #4993, #2170, .T. ) ;
#417 = ORIENTED_EDGE ( 'NONE', *, *, #4078, .F. ) ;
#418 = EDGE_CURVE ( 'NONE', #7308, #2028, #4397, .T. ) ;
#419 = EDGE_CURVE ( 'NONE', #6751, #183, #6215, .T. ) ;
#420 = AXIS2_PLACEMENT_3D ( 'NONE', #1513, #3788, #1169 ) ;
#421 = AXIS2_PLACEMENT_3D ( 'NONE', #5145, #5665, #2248 ) ;
#422 = CARTESIAN_POINT ( 'NONE',  ( -5.000000000000000888, -8.660254037844389075, -140.0000000000000284 ) ) ;
#423 = DIRECTION ( 'NONE',  ( 1.000000000000000000, 0.000000000000000000, 0.000000000000000000 ) ) ;
#424 = CARTESIAN_POINT ( 'NONE',  ( -10.00000000000000000, 0.000000000000000000, -140.0000000000000000 ) ) ;
#425 = DIRECTION ( 'NONE',  ( -1.000000000000000000, 0.000000000000000000, 0.000000000000000000 ) ) ;
#426 = ORIENTED_EDGE ( 'NONE', *, *, #4897, .F. ) ;
#427 = VECTOR ( 'NONE', #131, 1000.000000000000000 ) ;
#428 = DIRECTION ( 'NONE',  ( 0.5000000000000022204, 0.8660254037844374864, -0.000000000000000000 ) ) ;
#429 = MECHANICAL_DESIGN_GEOMETRIC_PRESENTATION_REPRESENTATION (  '', ( #5917 ), #4698 ) ;
#430 = EDGE_CURVE ( 'NONE', #5253, #5386, #3873, .T. ) ;
#431 = VERTEX_POINT ( 'NONE', #5361 ) ;
#432 = VERTEX_POINT ( 'NONE', #3020 ) ;
#433 = DIRECTION ( 'NONE',  ( -0.000000000000000000, 1.000000000000000000, -0.000000000000000000 ) ) ;
#434 = DIRECTION ( 'NONE',  ( -1.000000000000000000, 0.000000000000000000, -0.000000000000000000 ) ) ;
#435 = CARTESIAN_POINT ( 'NONE',  ( 25.00000000000000000, 0.000000000000000000, 2.055000000000000160 ) ) ;
#436 = CARTESIAN_POINT ( 'NONE',  ( -4.000000000000000000, 0.000000000000000000, 0.000000000000000000 ) ) ;
#437 = AXIS2_PLACEMENT_3D ( 'NONE', #4317, #2581, #917 ) ;
#438 = CARTESIAN_POINT ( 'NONE',  ( 219.9999999999999716, -20.00000000000000000, -165.1500000000000625 ) ) ;
#439 = AXIS2_PLACEMENT_3D ( 'NONE', #1753, #4533, #2236 ) ;
#440 = EDGE_CURVE ( 'NONE', #3349, #7332, #2788, .T. ) ;
#441 = ORIENTED_EDGE ( 'NONE', *, *, #1230, .T. ) ;
#442 = VECTOR ( 'NONE', #1696, 1000.000000000000114 ) ;
#443 = FACE_OUTER_BOUND ( 'NONE', #2972, .T. ) ;
#444 = CARTESIAN_POINT ( 'NONE',  ( 164.9999999999999716, 8.660254037844390851, 145.0000000000000284 ) ) ;
#445 = CARTESIAN_POINT ( 'NONE',  ( -1.828356344711647319, -3.563200125723192002, -1.076197711133951296E-14 ) ) ;
#446 = CARTESIAN_POINT ( 'NONE',  ( 285.0000000000000568, 8.660254037844390851, 140.0000000000000000 ) ) ;
#447 = AXIS2_PLACEMENT_3D ( 'NONE', #2275, #5736, #5768 ) ;
#448 = FILL_AREA_STYLE ('',( #957 ) ) ;
#449 =( REPRESENTATION_RELATIONSHIP ('NONE','NONE', #5587, #1193 ) REPRESENTATION_RELATIONSHIP_WITH_TRANSFORMATION ( #1154 )SHAPE_REPRESENTATION_RELATIONSHIP( ) );
#450 = VERTEX_POINT ( 'NONE', #1982 ) ;
#451 = ORIENTED_EDGE ( 'NONE', *, *, #5219, .F. ) ;
#453 = CIRCLE ( 'NONE', #2820, 2.649999999999985700 ) ;
#452 = DIRECTION ( 'NONE',  ( 0.000000000000000000, 0.000000000000000000, 1.000000000000000000 ) ) ;
#454 = EDGE_LOOP ( 'NONE', ( #6459, #72, #5565, #1387 ) ) ;
#455 = DIRECTION ( 'NONE',  ( 0.000000000000000000, 0.000000000000000000, -1.000000000000000000 ) ) ;
#456 = DIRECTION ( 'NONE',  ( 1.000000000000000000, 0.000000000000000000, -0.000000000000000000 ) ) ;
#457 = CARTESIAN_POINT ( 'NONE',  ( -5.000000000000000888, 8.660254037844390851, -150.0000000000000000 ) ) ;
#458 = ORIENTED_EDGE ( 'NONE', *, *, #67, .F. ) ;
#459 = AXIS2_PLACEMENT_3D ( 'NONE', #4842, #4603, #3459 ) ;
#460 = CARTESIAN_POINT ( 'NONE',  ( -30.00000000000002842, -20.00000000000000000, 200.0000000000000000 ) ) ;
#461 = B_SPLINE_CURVE_WITH_KNOTS ( 'NONE', 3,
 ( #1150, #4028, #622, #2880, #68 ),
 .UNSPECIFIED., .F., .F.,
 ( 4, 1, 4 ),
 ( 0.000000000000000000, 0.002309401076758505790, 0.004618802153517011580 ),
 .UNSPECIFIED. ) ;
#462 = EDGE_CURVE ( 'NONE', #1179, #5999, #4944, .T. ) ;
#463 = CARTESIAN_POINT ( 'NONE',  ( 0.000000000000000000, 5.051668046482832750E-16, -4.000000000000000000 ) ) ;
#464 = DIRECTION ( 'NONE',  ( -0.000000000000000000, 1.000000000000000000, -0.000000000000000000 ) ) ;
#465 = DIRECTION ( 'NONE',  ( 0.000000000000000000, 0.000000000000000000, -1.000000000000000000 ) ) ;
#466 = ORIENTED_EDGE ( 'NONE', *, *, #7136, .F. ) ;
#467 = LINE ( 'NONE', #1023, #7209 ) ;
#468 = VERTEX_POINT ( 'NONE', #1903 ) ;
#469 = ORIENTED_EDGE ( 'NONE', *, *, #956, .F. ) ;
#470 = CARTESIAN_POINT ( 'NONE',  ( 0.000000000000000000, 0.000000000000000000, 0.000000000000000000 ) ) ;
#471 = CARTESIAN_POINT ( 'NONE',  ( 2.500000000000000000, 2.357898499370433054, -1.951563910473907981E-15 ) ) ;
#472 = PLANE ( 'NONE',  #1920 ) ;
#473 = DIRECTION ( 'NONE',  ( 0.000000000000000000, 1.000000000000000000, 0.000000000000000000 ) ) ;
#474 = EDGE_CURVE ( 'NONE', #2018, #3309, #212, .T. ) ;
#475 = FACE_OUTER_BOUND ( 'NONE', #720, .T. ) ;
#476 = ORIENTED_EDGE ( 'NONE', *, *, #4916, .F. ) ;
#477 = LINE ( 'NONE', #3366, #540 ) ;
#478 = VERTEX_POINT ( 'NONE', #320 ) ;
#479 = FACE_BOUND ( 'NONE', #3779, .T. ) ;
#480 = DIRECTION ( 'NONE',  ( -1.000000000000000000, -0.000000000000000000, -0.000000000000000000 ) ) ;
#481 = CARTESIAN_POINT ( 'NONE',  ( 0.000000000000000000, 1.178949249685213863, -2.042000000000001148 ) ) ;
#482 = CARTESIAN_POINT ( 'NONE',  ( -2.000000000000001776, 0.000000000000000000, -13.29999999999999893 ) ) ;
#483 =( NAMED_UNIT ( * ) PLANE_ANGLE_UNIT ( ) SI_UNIT ( $, .RADIAN. ) );
#484 = EDGE_CURVE ( 'NONE', #3104, #5307, #4352, .T. ) ;
#485 = FACE_OUTER_BOUND ( 'NONE', #5786, .T. ) ;
#486 = ORIENTED_EDGE ( 'NONE', *, *, #2822, .F. ) ;
#487 = ADVANCED_FACE ( 'NONE', ( #5469 ), #2188, .T. ) ;
#488 = EDGE_LOOP ( 'NONE', ( #3716, #3762 ) ) ;
#489 = DIRECTION ( 'NONE',  ( 6.123233995736766036E-17, -1.000000000000000000, 0.000000000000000000 ) ) ;
#490 = ORIENTED_EDGE ( 'NONE', *, *, #2940, .T. ) ;
#491 = CARTESIAN_POINT ( 'NONE',  ( 435.0000000000000568, -8.660254037844389075, 145.0000000000000284 ) ) ;
#492 = LINE ( 'NONE', #3348, #3419 ) ;
#493 = ORIENTED_EDGE ( 'NONE', *, *, #3790, .T. ) ;
#494 = DIRECTION ( 'NONE',  ( -0.000000000000000000, -0.000000000000000000, 1.000000000000000000 ) ) ;
#495 = CARTESIAN_POINT ( 'NONE',  ( 0.000000000000000000, 0.000000000000000000, -121.0000000000000000 ) ) ;
#496 = DIRECTION ( 'NONE',  ( 0.000000000000000000, 0.000000000000000000, -1.000000000000000000 ) ) ;
#497 =( REPRESENTATION_RELATIONSHIP ('NONE','NONE', #5587, #951 ) REPRESENTATION_RELATIONSHIP_WITH_TRANSFORMATION ( #6339 )SHAPE_REPRESENTATION_RELATIONSHIP( ) );
#498 = EDGE_LOOP ( 'NONE', ( #4214, #3564, #961, #4905, #71 ) ) ;
#499 = CARTESIAN_POINT ( 'NONE',  ( -4.197393957002303999, 0.4069871074557429025, -3.503767560748926257 ) ) ;
#500 = EDGE_CURVE ( 'NONE', #4203, #1612, #4312, .T. ) ;
#501 = EDGE_LOOP ( 'NONE', ( #2407, #5320, #3926, #4754 ) ) ;
#502 = ORIENTED_EDGE ( 'NONE', *, *, #7249, .F. ) ;
#503 = LINE ( 'NONE', #3939, #965 ) ;
#504 = CARTESIAN_POINT ( 'NONE',  ( 3.540020015735602765, 2.810662092924382627, -3.602146406945867962 ) ) ;
#505 = CARTESIAN_POINT ( 'NONE',  ( 275.0000000000000000, 8.660254037844390851, 140.0000000000000000 ) ) ;
#506 = CARTESIAN_POINT ( 'NONE',  ( 1.800000000000002931, 0.000000000000000000, -13.50000000000000178 ) ) ;
#507 = CIRCLE ( 'NONE', #5271, 12.44999999999999929 ) ;
#508 = FACE_OUTER_BOUND ( 'NONE', #5725, .T. ) ;
#509 = LINE ( 'NONE', #3410, #7223 ) ;
#510 = ORIENTED_EDGE ( 'NONE', *, *, #4260, .T. ) ;
#511 = EDGE_CURVE ( 'NONE', #4692, #7233, #922, .T. ) ;
#512 = CARTESIAN_POINT ( 'NONE',  ( 25.00000000000000000, 0.000000000000000000, 0.000000000000000000 ) ) ;
#513 = LINE ( 'NONE', #4964, #4728 ) ;
#514 = LINE ( 'NONE', #2355, #1215 ) ;
#515 = FACE_BOUND ( 'NONE', #4736, .T. ) ;
#516 = DIRECTION ( 'NONE',  ( -0.000000000000000000, -0.000000000000000000, 1.000000000000000000 ) ) ;
#517 = AXIS2_PLACEMENT_3D ( 'NONE', #2143, #842, #1959 ) ;
#518 = EDGE_LOOP ( 'NONE', ( #824, #118 ) ) ;
#519 = EDGE_LOOP ( 'NONE', ( #3409, #1674, #1856, #6245 ) ) ;
#520 = COLOUR_RGB ( '',0.8941176470588234615, 0.8941176470588234615, 0.8941176470588234615 ) ;
#521 = EDGE_CURVE ( 'NONE', #1652, #1784, #3123, .T. ) ;
#522 = SHAPE_DEFINITION_REPRESENTATION ( #2401, #951 ) ;
#523 = ORIENTED_EDGE ( 'NONE', *, *, #7193, .F. ) ;
#524 = PLANE ( 'NONE',  #3519 ) ;
#525 = AXIS2_PLACEMENT_3D ( 'NONE', #3543, #4080, #2381 ) ;
#526 = DIRECTION ( 'NONE',  ( -0.000000000000000000, -1.000000000000000000, -0.000000000000000000 ) ) ;
#527 = ORIENTED_EDGE ( 'NONE', *, *, #701, .F. ) ;
#528 = CARTESIAN_POINT ( 'NONE',  ( 155.0000000000000000, 8.660254037844390851, 139.9990000000000236 ) ) ;
#529 = CARTESIAN_POINT ( 'NONE',  ( 235.0000000000000000, 8.660254037844390851, 140.0000000000000000 ) ) ;
#530 = AXIS2_PLACEMENT_3D ( 'NONE', #1311, #5247, #5852 ) ;
#531 = DIRECTION ( 'NONE',  ( 0.000000000000000000, -1.000000000000000000, 0.000000000000000000 ) ) ;
#532 = VECTOR ( 'NONE', #4257, 1000.000000000000000 ) ;
#533 = DIRECTION ( 'NONE',  ( 0.000000000000000000, 0.000000000000000000, 1.000000000000000000 ) ) ;
#534 = ORIENTED_EDGE ( 'NONE', *, *, #6574, .T. ) ;
#535 = DIRECTION ( 'NONE',  ( 0.000000000000000000, 1.000000000000000000, 0.000000000000000000 ) ) ;
#536 = ADVANCED_FACE ( 'NONE', ( #4765 ), #3613, .T. ) ;
#537 = AXIS2_PLACEMENT_3D ( 'NONE', #2124, #3352, #7303 ) ;
#538 = LINE ( 'NONE', #6204, #2789 ) ;
#539 = AXIS2_PLACEMENT_3D ( 'NONE', #7178, #4930, #2078 ) ;
#540 = VECTOR ( 'NONE', #6836, 1000.000000000000000 ) ;
#541 = VERTEX_POINT ( 'NONE', #1871 ) ;
#542 = LINE ( 'NONE', #49, #3343 ) ;
#543 = DIRECTION ( 'NONE',  ( 1.000000000000000000, 0.000000000000000000, 0.000000000000000000 ) ) ;
#544 = CARTESIAN_POINT ( 'NONE',  ( 2.500000000000000000, -1.768423874527823791, -1.020999999999998353 ) ) ;
#545 = DIRECTION ( 'NONE',  ( 1.000000000000000000, 0.000000000000000000, 0.000000000000000000 ) ) ;
#546 = AXIS2_PLACEMENT_3D ( 'NONE', #3740, #473, #7159 ) ;
#547 = STYLED_ITEM ( 'NONE', ( #4320 ), #5754 ) ;
#548 = ORIENTED_EDGE ( 'NONE', *, *, #7125, .F. ) ;
#549 = CARTESIAN_POINT ( 'NONE',  ( 4.204015924366189871, -1.626724848190933548, -3.610627190413393084 ) ) ;
#550 = ORIENTED_EDGE ( 'NONE', *, *, #6741, .T. ) ;
#551 = VECTOR ( 'NONE', #6256, 1000.000000000000000 ) ;
#552 = AXIS2_PLACEMENT_3D ( 'NONE', #1450, #3727, #6555 ) ;
#553 = FACE_OUTER_BOUND ( 'NONE', #3654, .T. ) ;
#554 = CARTESIAN_POINT ( 'NONE',  ( 303.3333333333333144, -14.99999999999999822, 162.5000000000000853 ) ) ;
#555 = CARTESIAN_POINT ( 'NONE',  ( 4.211140560182196957, -2.431303136016555122, -3.745885042887436622 ) ) ;
#556 = EDGE_CURVE ( 'NONE', #1367, #3466, #7089, .T. ) ;
#557 = CIRCLE ( 'NONE', #6773, 0.5155456020628804703 ) ;
#558 = PRESENTATION_STYLE_ASSIGNMENT (( #3449 ) ) ;
#559 = VECTOR ( 'NONE', #1074, 1000.000000000000000 ) ;
#560 = ORIENTED_EDGE ( 'NONE', *, *, #3390, .T. ) ;
#561 = EDGE_LOOP ( 'NONE', ( #5979, #4892 ) ) ;
#562 = DIRECTION ( 'NONE',  ( 0.000000000000000000, 0.000000000000000000, 1.000000000000000000 ) ) ;
#563 = VERTEX_POINT ( 'NONE', #6568 ) ;
#564 = VECTOR ( 'NONE', #6045, 1000.000000000000000 ) ;
#565 = PRODUCT_DEFINITION_SHAPE ( 'NONE', 'NONE',  #7382 ) ;
#566 = CARTESIAN_POINT ( 'NONE',  ( -11.00000000000000000, 0.000000000000000000, 121.0000000000000000 ) ) ;
#567 = ADVANCED_FACE ( 'NONE', ( #2014 ), #1429, .T. ) ;
#568 = DIRECTION ( 'NONE',  ( 1.000000000000000000, 0.000000000000000000, 0.000000000000000000 ) ) ;
#569 = AXIS2_PLACEMENT_3D ( 'NONE', #2262, #6216, #568 ) ;
#570 = ORIENTED_EDGE ( 'NONE', *, *, #1823, .T. ) ;
#571 = DIRECTION ( 'NONE',  ( 1.000000000000000000, 0.000000000000000000, 0.000000000000000000 ) ) ;
#572 = CARTESIAN_POINT ( 'NONE',  ( -5.000000000000000888, 8.660254037844390851, 150.0000000000000000 ) ) ;
#573 = VECTOR ( 'NONE', #3455, 1000.000000000000000 ) ;
#574 = DIRECTION ( 'NONE',  ( 0.000000000000000000, 0.000000000000000000, -1.000000000000000000 ) ) ;
#575 = EDGE_CURVE ( 'NONE', #1949, #4530, #5787, .T. ) ;
#576 = ORIENTED_EDGE ( 'NONE', *, *, #6862, .T. ) ;
#577 = LINE ( 'NONE', #6259, #6396 ) ;
#578 = ORIENTED_EDGE ( 'NONE', *, *, #7274, .F. ) ;
#579 = DIRECTION ( 'NONE',  ( -0.000000000000000000, 1.000000000000000000, -0.000000000000000000 ) ) ;
#580 = CARTESIAN_POINT ( 'NONE',  ( -4.197393957002303999, -7.773935952363655451E-14, -3.503767560748929810 ) ) ;
#581 = CONTEXT_DEPENDENT_SHAPE_REPRESENTATION ( #6235, #6353 ) ;
#582 = CARTESIAN_POINT ( 'NONE',  ( 136.6666666666666288, -20.00000000000000000, 162.5000000000000853 ) ) ;
#583 = DIRECTION ( 'NONE',  ( 0.000000000000000000, 0.000000000000000000, -1.000000000000000000 ) ) ;
#584 = VERTEX_POINT ( 'NONE', #1395 ) ;
#585 = DIRECTION ( 'NONE',  ( 0.000000000000000000, 0.000000000000000000, -1.000000000000000000 ) ) ;
#586 = VERTEX_POINT ( 'NONE', #3703 ) ;
#587 = DIRECTION ( 'NONE',  ( -0.000000000000000000, 1.000000000000000000, -0.000000000000000000 ) ) ;
#588 = CARTESIAN_POINT ( 'NONE',  ( 386.6666666666666288, -14.99999999999999822, 162.5000000000000853 ) ) ;
#589 = LINE ( 'NONE', #3742, #4186 ) ;
#590 = CARTESIAN_POINT ( 'NONE',  ( 4.999999999999999112, 8.660254037844390851, -150.0000000000000000 ) ) ;
#591 = ORIENTED_EDGE ( 'NONE', *, *, #1590, .T. ) ;
#592 = ORIENTED_EDGE ( 'NONE', *, *, #1151, .F. ) ;
#593 = EDGE_CURVE ( 'NONE', #7027, #310, #2577, .T. ) ;
#594 = DIRECTION ( 'NONE',  ( 0.000000000000000000, 0.000000000000000000, 1.000000000000000000 ) ) ;
#595 = ORIENTED_EDGE ( 'NONE', *, *, #5293, .F. ) ;
#596 = LINE ( 'NONE', #3885, #190 ) ;
#597 = CARTESIAN_POINT ( 'NONE',  ( -5.000000000000000888, 0.000000000000000000, 140.0000000000000000 ) ) ;
#598 = VERTEX_POINT ( 'NONE', #834 ) ;
#599 = ADVANCED_FACE ( 'NONE', ( #4872 ), #1488, .T. ) ;
#600 = DIRECTION ( 'NONE',  ( -0.000000000000000000, -1.000000000000000000, -0.000000000000000000 ) ) ;
#601 = CARTESIAN_POINT ( 'NONE',  ( 470.0000000000000000, -15.00000000000000000, 145.0000000000000284 ) ) ;
#602 = ADVANCED_FACE ( 'NONE', ( #279 ), #4481, .T. ) ;
#603 = DIRECTION ( 'NONE',  ( 0.000000000000000000, 0.000000000000000000, 1.000000000000000000 ) ) ;
#604 = EDGE_LOOP ( 'NONE', ( #960, #1830, #4158, #6314 ) ) ;
#605 = CARTESIAN_POINT ( 'NONE',  ( -4.207491450040567571, 2.029819825146470524, -3.671670828759566074 ) ) ;
#606 = ORIENTED_EDGE ( 'NONE', *, *, #2840, .T. ) ;
#607 = AXIS2_PLACEMENT_3D ( 'NONE', #5873, #2374, #227 ) ;
#608 = ADVANCED_FACE ( 'NONE', ( #5617 ), #1013, .T. ) ;
#609 = LINE ( 'NONE', #1723, #1679 ) ;
#610 = CARTESIAN_POINT ( 'NONE',  ( 0.000000000000000000, 1.178949249685218525, 2.041999999999999371 ) ) ;
#611 = CARTESIAN_POINT ( 'NONE',  ( -5.000000000000000888, -8.660254037844389075, 150.0000000000000000 ) ) ;
#612 = ORIENTED_EDGE ( 'NONE', *, *, #6327, .F. ) ;
#613 = ADVANCED_FACE ( 'NONE', ( #47 ), #1091, .F. ) ;
#614 = CARTESIAN_POINT ( 'NONE',  ( 4.197393957002303999, 7.772902908466098641E-14, -3.503767560748929810 ) ) ;
#615 = EDGE_LOOP ( 'NONE', ( #7175, #5759 ) ) ;
#616 = PRODUCT_DEFINITION_SHAPE ( 'NONE', 'NONE',  #7393 ) ;
#617 = DIRECTION ( 'NONE',  ( -1.000000000000000000, 0.000000000000000000, 0.000000000000000000 ) ) ;
#618 = PLANE ( 'NONE',  #6780 ) ;
#619 = CARTESIAN_POINT ( 'NONE',  ( -4.000000000000000000, 2.309401076758498483, -5.000000000000000000 ) ) ;
#620 = DIRECTION ( 'NONE',  ( -0.5000000000000051070, 0.000000000000000000, 0.8660254037844355990 ) ) ;
#621 = AXIS2_PLACEMENT_3D ( 'NONE', #5510, #4279, #4360 ) ;
#622 = CARTESIAN_POINT ( 'NONE',  ( -4.000000000000000000, -7.806255641895631925E-15, -3.142992957459232350 ) ) ;
#623 = EDGE_CURVE ( 'NONE', #1976, #3497, #2947, .T. ) ;
#624 = ORIENTED_EDGE ( 'NONE', *, *, #6068, .T. ) ;
#625 = SHAPE_DEFINITION_REPRESENTATION ( #940, #4771 ) ;
#626 = ORIENTED_EDGE ( 'NONE', *, *, #2507, .F. ) ;
#627 = ADVANCED_FACE ( 'NONE', ( #4608 ), #12, .F. ) ;
#628 = DIRECTION ( 'NONE',  ( 0.000000000000000000, 0.000000000000000000, 1.000000000000000000 ) ) ;
#629 = CARTESIAN_POINT ( 'NONE',  ( -4.000000000000000000, 1.700094919196744270, -3.320312364301766017 ) ) ;
#630 = VERTEX_POINT ( 'NONE', #2832 ) ;
#631 =( REPRESENTATION_RELATIONSHIP ('NONE','NONE', #5587, #951 ) REPRESENTATION_RELATIONSHIP_WITH_TRANSFORMATION ( #3671 )SHAPE_REPRESENTATION_RELATIONSHIP( ) );
#632 = CIRCLE ( 'NONE', #7087, 19.00000000000000000 ) ;
#633 = CARTESIAN_POINT ( 'NONE',  ( 0.000000000000000000, 0.000000000000000000, 140.0000000000000000 ) ) ;
#634 = LINE ( 'NONE', #149, #4836 ) ;
#635 = EDGE_CURVE ( 'NONE', #3059, #1111, #1755, .T. ) ;
#636 = ORIENTED_EDGE ( 'NONE', *, *, #5776, .F. ) ;
#637 = DIRECTION ( 'NONE',  ( -1.000000000000000000, 0.000000000000000000, 0.000000000000000000 ) ) ;
#638 = EDGE_CURVE ( 'NONE', #5460, #3234, #3393, .T. ) ;
#639 = ORIENTED_EDGE ( 'NONE', *, *, #6547, .F. ) ;
#640 = AXIS2_PLACEMENT_3D ( 'NONE', #2848, #6942, #1184 ) ;
#641 = ORIENTED_EDGE ( 'NONE', *, *, #1393, .T. ) ;
#642 = VECTOR ( 'NONE', #4176, 1000.000000000000000 ) ;
#643 = DIRECTION ( 'NONE',  ( 0.000000000000000000, 0.000000000000000000, -1.000000000000000000 ) ) ;
#644 = LINE ( 'NONE', #2899, #2333 ) ;
#645 = CARTESIAN_POINT ( 'NONE',  ( 235.0000000000000000, 8.660254037844390851, 139.9990000000000236 ) ) ;
#646 = FACE_OUTER_BOUND ( 'NONE', #5518, .T. ) ;
#647 = VERTEX_POINT ( 'NONE', #6436 ) ;
#648 = EDGE_CURVE ( 'NONE', #4019, #2725, #2787, .T. ) ;
#649 = CARTESIAN_POINT ( 'NONE',  ( -2.000000000000001776, 0.000000000000000000, -12.77500000000000036 ) ) ;
#650 = AXIS2_PLACEMENT_3D ( 'NONE', #2212, #6051, #988 ) ;
#651 = VECTOR ( 'NONE', #2504, 1000.000000000000000 ) ;
#652 = EDGE_CURVE ( 'NONE', #2249, #3158, #5654, .T. ) ;
#653 = ORIENTED_EDGE ( 'NONE', *, *, #416, .T. ) ;
#654 = LINE ( 'NONE', #7017, #3221 ) ;
#655 = CARTESIAN_POINT ( 'NONE',  ( -31.74999999999995737, 0.000000000000000000, 0.000000000000000000 ) ) ;
#656 = AXIS2_PLACEMENT_3D ( 'NONE', #3631, #4731, #1283 ) ;
#657 = AXIS2_PLACEMENT_3D ( 'NONE', #6929, #4215, #1855 ) ;
#658 = DIRECTION ( 'NONE',  ( 0.000000000000000000, 0.000000000000000000, -1.000000000000000000 ) ) ;
#659 = DIRECTION ( 'NONE',  ( 0.000000000000000000, 1.000000000000000000, 0.000000000000000000 ) ) ;
#660 = EDGE_CURVE ( 'NONE', #6352, #1004, #181, .T. ) ;
#661 = AXIS2_PLACEMENT_3D ( 'NONE', #7149, #4263, #2002 ) ;
#662 = COLOUR_RGB ( '',0.8941176470588234615, 0.8941176470588234615, 0.8941176470588234615 ) ;
#663 = ORIENTED_EDGE ( 'NONE', *, *, #1944, .F. ) ;
#664 = ORIENTED_EDGE ( 'NONE', *, *, #319, .T. ) ;
#665 = DIRECTION ( 'NONE',  ( -1.000000000000000000, 0.000000000000000000, 0.000000000000000000 ) ) ;
#666 = LINE ( 'NONE', #6392, #5923 ) ;
#667 = EDGE_LOOP ( 'NONE', ( #840, #4739, #1362, #2962 ) ) ;
#668 = VECTOR ( 'NONE', #3036, 1000.000000000000000 ) ;
#669 = CARTESIAN_POINT ( 'NONE',  ( 435.0000000000000568, 8.660254037844390851, 139.9990000000000236 ) ) ;
#670 = STYLED_ITEM ( 'NONE', ( #5899 ), #1370 ) ;
#671 = ORIENTED_EDGE ( 'NONE', *, *, #5764, .F. ) ;
#672 = AXIS2_PLACEMENT_3D ( 'NONE', #2662, #4518, #2775 ) ;
#673 = CARTESIAN_POINT ( 'NONE',  ( 2.000000000000001776, 0.000000000000000000, 0.000000000000000000 ) ) ;
#674 = CARTESIAN_POINT ( 'NONE',  ( -30.00000000000002842, -20.00000000000000000, 200.0000000000000000 ) ) ;
#675 = CIRCLE ( 'NONE', #5109, 2.649999999999985700 ) ;
#676 = CARTESIAN_POINT ( 'NONE',  ( -4.000000000000000000, 2.309401076758498483, -3.433295621305379353 ) ) ;
#677 = LINE ( 'NONE', #3608, #2568 ) ;
#678 = APPLICATION_CONTEXT ( 'automotive_design' ) ;
#679 = EDGE_LOOP ( 'NONE', ( #1531, #1316, #1080, #4303 ) ) ;
#680 = EDGE_CURVE ( 'NONE', #5556, #1411, #5423, .T. ) ;
#681 = DIRECTION ( 'NONE',  ( 1.000000000000000000, 0.000000000000000000, 0.000000000000000000 ) ) ;
#682 = MECHANICAL_DESIGN_GEOMETRIC_PRESENTATION_REPRESENTATION (  '', ( #6426 ), #3527 ) ;
#683 = CARTESIAN_POINT ( 'NONE',  ( 219.9999999999999716, -15.00000000000000000, 159.8500000000001080 ) ) ;
#684 = PLANE ( 'NONE',  #1220 ) ;
#685 = CARTESIAN_POINT ( 'NONE',  ( 205.0000000000000284, -8.660254037844389075, 140.0000000000000000 ) ) ;
#686 =( NAMED_UNIT ( * ) SI_UNIT ( $, .STERADIAN. ) SOLID_ANGLE_UNIT ( ) );
#687 = ORIENTED_EDGE ( 'NONE', *, *, #4021, .F. ) ;
#688 = DIRECTION ( 'NONE',  ( 1.000000000000000000, 0.000000000000000000, 0.000000000000000000 ) ) ;
#689 = ORIENTED_EDGE ( 'NONE', *, *, #5366, .F. ) ;
#690 = CARTESIAN_POINT ( 'NONE',  ( 275.0000000000000000, 8.660254037844390851, 139.9990000000000236 ) ) ;
#691 = DIRECTION ( 'NONE',  ( -0.000000000000000000, 0.8660254037844390407, 0.4999999999999993339 ) ) ;
#692 = DIRECTION ( 'NONE',  ( 0.000000000000000000, 0.000000000000000000, 1.000000000000000000 ) ) ;
#693 = CARTESIAN_POINT ( 'NONE',  ( -2.000000000000006661, 3.464101615137750834, 0.000000000000000000 ) ) ;
#694 = EDGE_CURVE ( 'NONE', #7258, #2062, #2271, .T. ) ;
#695 = DIRECTION ( 'NONE',  ( 0.000000000000000000, 0.000000000000000000, 1.000000000000000000 ) ) ;
#696 = ORIENTED_EDGE ( 'NONE', *, *, #5063, .T. ) ;
#697 = EDGE_LOOP ( 'NONE', ( #5882, #6378, #4879, #7072 ) ) ;
#698 = PRODUCT_DEFINITION_SHAPE ( 'NONE', 'NONE',  #7343 ) ;
#699 = DIRECTION ( 'NONE',  ( -1.000000000000000000, 0.000000000000000000, 0.000000000000000000 ) ) ;
#700 = ORIENTED_EDGE ( 'NONE', *, *, #329, .T. ) ;
#701 = EDGE_CURVE ( 'NONE', #2491, #3982, #2202, .T. ) ;
#702 = LINE ( 'NONE', #1658, #4364 ) ;
#703 = CARTESIAN_POINT ( 'NONE',  ( 470.0000000000000000, 15.00000000000000000, 145.0000000000000284 ) ) ;
#704 = ORIENTED_EDGE ( 'NONE', *, *, #4059, .T. ) ;
#705 = CARTESIAN_POINT ( 'NONE',  ( -3.355112389629170799, 2.681727112203152963, -0.2256878752776689534 ) ) ;
#706 = DIRECTION ( 'NONE',  ( 0.000000000000000000, 1.000000000000000000, 0.000000000000000000 ) ) ;
#707 = FACE_OUTER_BOUND ( 'NONE', #3501, .T. ) ;
#708 = DIRECTION ( 'NONE',  ( 0.000000000000000000, -1.000000000000000000, 0.000000000000000000 ) ) ;
#709 = VERTEX_POINT ( 'NONE', #3935 ) ;
#710 = DIRECTION ( 'NONE',  ( 0.000000000000000000, 0.5000000000000011102, 0.8660254037844380415 ) ) ;
#711 = FACE_OUTER_BOUND ( 'NONE', #4712, .T. ) ;
#712 = CONTEXT_DEPENDENT_SHAPE_REPRESENTATION ( #3825, #5155 ) ;
#713 = DIRECTION ( 'NONE',  ( -1.000000000000000000, 0.000000000000000000, -0.000000000000000000 ) ) ;
#714 = CARTESIAN_POINT ( 'NONE',  ( 0.000000000000000000, 0.000000000000000000, -121.0000000000000000 ) ) ;
#715 = EDGE_LOOP ( 'NONE', ( #2151, #1356, #4570, #1862 ) ) ;
#716 = CYLINDRICAL_SURFACE ( 'NONE', #2053, 2.100000000000000089 ) ;
#717 = EDGE_CURVE ( 'NONE', #5864, #5089, #2077, .T. ) ;
#718 = UNCERTAINTY_MEASURE_WITH_UNIT (LENGTH_MEASURE( 1.000000000000000082E-05 ), #3530, 'distance_accuracy_value', 'NONE');
#719 = VERTEX_POINT ( 'NONE', #3399 ) ;
#720 = EDGE_LOOP ( 'NONE', ( #4664, #4216, #5470 ) ) ;
#721 = DIRECTION ( 'NONE',  ( 0.000000000000000000, 0.000000000000000000, -1.000000000000000000 ) ) ;
#722 = CARTESIAN_POINT ( 'NONE',  ( -4.236525694536558362, 2.416953475386465211, -3.751298745799836354 ) ) ;
#723 = DIRECTION ( 'NONE',  ( -0.000000000000000000, 1.000000000000000000, -0.000000000000000000 ) ) ;
#724 = DIRECTION ( 'NONE',  ( 0.000000000000000000, -0.5000000000000011102, -0.8660254037844379305 ) ) ;
#725 = VECTOR ( 'NONE', #6797, 1000.000000000000000 ) ;
#726 = DIRECTION ( 'NONE',  ( 0.000000000000000000, 0.000000000000000000, 1.000000000000000000 ) ) ;
#727 = EDGE_CURVE ( 'NONE', #2273, #3217, #1357, .T. ) ;
#728 = EDGE_CURVE ( 'NONE', #7155, #3466, #4536, .T. ) ;
#729 = ORIENTED_EDGE ( 'NONE', *, *, #2396, .T. ) ;
#730 = VECTOR ( 'NONE', #6726, 1000.000000000000000 ) ;
#731 = DIRECTION ( 'NONE',  ( -0.000000000000000000, 0.000000000000000000, 1.000000000000000000 ) ) ;
#732 = VERTEX_POINT ( 'NONE', #3972 ) ;
#733 = AXIS2_PLACEMENT_3D ( 'NONE', #3013, #238, #4760 ) ;
#734 = CARTESIAN_POINT ( 'NONE',  ( -4.000000000000000000, -1.680117682357936904, -3.316611593218794951 ) ) ;
#735 = EDGE_CURVE ( 'NONE', #3068, #3709, #577, .T. ) ;
#736 = ORIENTED_EDGE ( 'NONE', *, *, #635, .F. ) ;
#737 = LINE ( 'NONE', #1881, #668 ) ;
#738 = VECTOR ( 'NONE', #3505, 1000.000000000000000 ) ;
#739 = ORIENTED_EDGE ( 'NONE', *, *, #5593, .F. ) ;
#740 = ADVANCED_FACE ( 'NONE', ( #1129 ), #5700, .F. ) ;
#741 = ORIENTED_EDGE ( 'NONE', *, *, #4255, .F. ) ;
#742 = VECTOR ( 'NONE', #3862, 1000.000000000000000 ) ;
#743 = LINE ( 'NONE', #3044, #5257 ) ;
#744 = CYLINDRICAL_SURFACE ( 'NONE', #7079, 11.05000000000000071 ) ;
#745 = FACE_OUTER_BOUND ( 'NONE', #2106, .T. ) ;
#746 = EDGE_CURVE ( 'NONE', #3709, #5646, #7108, .T. ) ;
#747 = ORIENTED_EDGE ( 'NONE', *, *, #1925, .T. ) ;
#748 = LINE ( 'NONE', #4722, #3999 ) ;
#749 = ORIENTED_EDGE ( 'NONE', *, *, #6006, .T. ) ;
#750 = ORIENTED_EDGE ( 'NONE', *, *, #175, .F. ) ;
#751 = DIRECTION ( 'NONE',  ( 0.000000000000000000, -0.000000000000000000, -1.000000000000000000 ) ) ;
#752 = CARTESIAN_POINT ( 'NONE',  ( -1.287237434361707233, -3.875615274277397937, -3.430618716626816500 ) ) ;
#753 = DIRECTION ( 'NONE',  ( 0.000000000000000000, 0.000000000000000000, -1.000000000000000000 ) ) ;
#754 = CARTESIAN_POINT ( 'NONE',  ( -0.6507732100473471171, 4.243078065514775510, -0.2236248678334823436 ) ) ;
#755 = AXIS2_PLACEMENT_3D ( 'NONE', #1285, #4088, #6492 ) ;
#756 = AXIS2_PLACEMENT_3D ( 'NONE', #2798, #5102, #1824 ) ;
#757 = CIRCLE ( 'NONE', #6087, 11.05000000000000071 ) ;
#758 = AXIS2_PLACEMENT_3D ( 'NONE', #4531, #139, #4493 ) ;
#759 = DIRECTION ( 'NONE',  ( 0.000000000000000000, -0.5000000000000012212, -0.8660254037844380415 ) ) ;
#760 = DIRECTION ( 'NONE',  ( 1.000000000000000000, 0.000000000000000000, 0.000000000000000000 ) ) ;
#761 = ORIENTED_EDGE ( 'NONE', *, *, #5228, .T. ) ;
#762 = PRODUCT_DEFINITION_FORMATION_WITH_SPECIFIED_SOURCE ( 'ANY', '', #3604, .NOT_KNOWN. ) ;
#763 = VERTEX_POINT ( 'NONE', #2931 ) ;
#764 = AXIS2_PLACEMENT_3D ( 'NONE', #2213, #6804, #3945 ) ;
#765 = CONTEXT_DEPENDENT_SHAPE_REPRESENTATION ( #1638, #2059 ) ;
#766 = CARTESIAN_POINT ( 'NONE',  ( 3.861362476283255685, 2.629030857715988656, -3.671615880910370500 ) ) ;
#767 = VERTEX_POINT ( 'NONE', #2448 ) ;
#768 = EDGE_CURVE ( 'NONE', #1382, #2446, #4670, .T. ) ;
#769 =( REPRESENTATION_RELATIONSHIP ('NONE','NONE', #5587, #951 ) REPRESENTATION_RELATIONSHIP_WITH_TRANSFORMATION ( #1255 )SHAPE_REPRESENTATION_RELATIONSHIP( ) );
#770 = AXIS2_PLACEMENT_3D ( 'NONE', #1738, #3448, #5781 ) ;
#771 = DIRECTION ( 'NONE',  ( -0.000000000000000000, -0.000000000000000000, 1.000000000000000000 ) ) ;
#772 = UNCERTAINTY_MEASURE_WITH_UNIT (LENGTH_MEASURE( 1.000000000000000082E-05 ), #4843, 'distance_accuracy_value', 'NONE');
#773 = ORIENTED_EDGE ( 'NONE', *, *, #4795, .T. ) ;
#774 = VECTOR ( 'NONE', #4510, 1000.000000000000000 ) ;
#775 = ORIENTED_EDGE ( 'NONE', *, *, #1901, .F. ) ;
#776 = VECTOR ( 'NONE', #5437, 1000.000000000000000 ) ;
#777 = CARTESIAN_POINT ( 'NONE',  ( 355.0000000000000000, 8.660254037844390851, 140.0000000000000000 ) ) ;
#778 = EDGE_CURVE ( 'NONE', #2792, #2671, #5384, .T. ) ;
#779 = ORIENTED_EDGE ( 'NONE', *, *, #4287, .T. ) ;
#780 = AXIS2_PLACEMENT_3D ( 'NONE', #2339, #3531, #2993 ) ;
#781 = SURFACE_STYLE_FILL_AREA ( #3533 ) ;
#782 = AXIS2_PLACEMENT_3D ( 'NONE', #1402, #5977, #5942 ) ;
#783 = ORIENTED_EDGE ( 'NONE', *, *, #4897, .T. ) ;
#784 = CARTESIAN_POINT ( 'NONE',  ( 0.000000000000000000, 0.000000000000000000, -4.974599999999998801 ) ) ;
#785 = ITEM_DEFINED_TRANSFORMATION ( 'NONE', 'NONE', #6030,  #1963 ) ;
#786 = DIRECTION ( 'NONE',  ( -0.000000000000000000, -1.000000000000000000, -0.000000000000000000 ) ) ;
#787 = DIRECTION ( 'NONE',  ( 1.000000000000000000, 0.000000000000000000, 0.000000000000000000 ) ) ;
#788 = ADVANCED_FACE ( 'NONE', ( #5803 ), #2341, .F. ) ;
#789 = AXIS2_PLACEMENT_3D ( 'NONE', #2244, #6905, #6338 ) ;
#790 = DIRECTION ( 'NONE',  ( 0.000000000000000000, 0.000000000000000000, 1.000000000000000000 ) ) ;
#791 = ORIENTED_EDGE ( 'NONE', *, *, #2057, .T. ) ;
#792 = B_SPLINE_CURVE_WITH_KNOTS ( 'NONE', 3,
 ( #3200, #6640, #861, #4950, #5387, #5546 ),
 .UNSPECIFIED., .F., .F.,
 ( 4, 2, 4 ),
 ( 0.003358874760055551890, 0.004541967308452098118, 0.005725059856848645212 ),
 .UNSPECIFIED. ) ;
#793 = CARTESIAN_POINT ( 'NONE',  ( -30.00000000000002842, -20.00000000000000000, 200.0000000000000000 ) ) ;
#794 = MANIFOLD_SOLID_BREP ( 'Boss-Extrude2', #5074 ) ;
#795 = ORIENTED_EDGE ( 'NONE', *, *, #7297, .F. ) ;
#796 = AXIS2_PLACEMENT_3D ( 'NONE', #1331, #817, #2406 ) ;
#797 = PRODUCT_DEFINITION_SHAPE ( 'NONE', 'NONE',  #7397 ) ;
#798 = EDGE_LOOP ( 'NONE', ( #259, #1754, #103, #7151, #5288 ) ) ;
#799 = CARTESIAN_POINT ( 'NONE',  ( 136.6666666666666288, -20.00000000000000000, -162.5000000000000853 ) ) ;
#800 = CARTESIAN_POINT ( 'NONE',  ( 0.000000000000000000, 1.438959988998140160E-15, -11.75000000000000000 ) ) ;
#801 = CARTESIAN_POINT ( 'NONE',  ( 0.000000000000000000, -1.178949249685213863, 2.042000000000002924 ) ) ;
#802 = CARTESIAN_POINT ( 'NONE',  ( 53.33333333333330017, -25.00000000000000000, -159.8500000000001080 ) ) ;
#803 = DIRECTION ( 'NONE',  ( 0.000000000000000000, 1.000000000000000000, 0.000000000000000000 ) ) ;
#804 = CARTESIAN_POINT ( 'NONE',  ( -3.264650091097280831E-13, -4.796980096169642493, -3.721999068284424617 ) ) ;
#805 = ORIENTED_EDGE ( 'NONE', *, *, #5847, .F. ) ;
#806 = CARTESIAN_POINT ( 'NONE',  ( 35.00000000000000000, 8.660254037844390851, 145.0000000000000284 ) ) ;
#807 = VERTEX_POINT ( 'NONE', #5838 ) ;
#808 = CARTESIAN_POINT ( 'NONE',  ( 53.33333333333330017, -20.00000000000000000, -162.5000000000000853 ) ) ;
#809 = EDGE_CURVE ( 'NONE', #1731, #4768, #4779, .T. ) ;
#810 = ORIENTED_EDGE ( 'NONE', *, *, #3072, .F. ) ;
#811 = EDGE_LOOP ( 'NONE', ( #6572, #6291, #4914, #5894 ) ) ;
#812 = LINE ( 'NONE', #2511, #1454 ) ;
#813 = PRODUCT_DEFINITION_SHAPE ( 'NONE', 'NONE',  #7344 ) ;
#814 = LINE ( 'NONE', #4326, #5802 ) ;
#815 = DIRECTION ( 'NONE',  ( -1.000000000000000000, -0.000000000000000000, -0.000000000000000000 ) ) ;
#816 = ORIENTED_EDGE ( 'NONE', *, *, #3949, .T. ) ;
#817 = DIRECTION ( 'NONE',  ( -0.000000000000000000, -1.000000000000000000, -0.000000000000000000 ) ) ;
#818 = VERTEX_POINT ( 'NONE', #2961 ) ;
#819 = EDGE_CURVE ( 'NONE', #4268, #3509, #677, .T. ) ;
#820 = LINE ( 'NONE', #2560, #5650 ) ;
#821 = CARTESIAN_POINT ( 'NONE',  ( 0.000000000000000000, 0.000000000000000000, 125.0000000000000000 ) ) ;
#822 = DIRECTION ( 'NONE',  ( -0.000000000000000000, 1.000000000000000000, -0.000000000000000000 ) ) ;
#823 = SURFACE_STYLE_USAGE ( .BOTH. , #1821 ) ;
#824 = ORIENTED_EDGE ( 'NONE', *, *, #1455, .F. ) ;
#825 = CARTESIAN_POINT ( 'NONE',  ( 75.00000000000001421, -8.660254037844389075, 140.0000000000000000 ) ) ;
#826 = ADVANCED_FACE ( 'NONE', ( #5951 ), #5268, .F. ) ;
#827 = ORIENTED_EDGE ( 'NONE', *, *, #4703, .F. ) ;
#828 = VERTEX_POINT ( 'NONE', #1883 ) ;
#829 = CARTESIAN_POINT ( 'NONE',  ( -3.540020015735593439, -2.810662092924100630, -3.602146406945814672 ) ) ;
#830 = FACE_OUTER_BOUND ( 'NONE', #3358, .T. ) ;
#831 = CARTESIAN_POINT ( 'NONE',  ( 0.000000000000000000, 0.000000000000000000, -0.2800830152838844622 ) ) ;
#832 = ADVANCED_FACE ( 'NONE', ( #191 ), #117, .T. ) ;
#833 = CARTESIAN_POINT ( 'NONE',  ( 1.800000000000001155, 1.628780242865979758E-15, 13.29999999999999893 ) ) ;
#834 = CARTESIAN_POINT ( 'NONE',  ( 25.00000000000000000, 0.000000000000000000, 2.055000000000000160 ) ) ;
#835 = ORIENTED_EDGE ( 'NONE', *, *, #5690, .T. ) ;
#836 = DIRECTION ( 'NONE',  ( -1.000000000000000000, 0.000000000000000000, 0.000000000000000000 ) ) ;
#837 = EDGE_LOOP ( 'NONE', ( #3025, #4554, #2784, #5893 ) ) ;
#838 = SURFACE_STYLE_FILL_AREA ( #2297 ) ;
#839 = DIRECTION ( 'NONE',  ( 0.000000000000000000, -0.000000000000000000, 1.000000000000000000 ) ) ;
#840 = ORIENTED_EDGE ( 'NONE', *, *, #4441, .F. ) ;
#841 = VERTEX_POINT ( 'NONE', #6475 ) ;
#842 = DIRECTION ( 'NONE',  ( 0.000000000000000000, 1.000000000000000000, 0.000000000000000000 ) ) ;
#843 = CARTESIAN_POINT ( 'NONE',  ( -4.000000000000000888, -2.309401076758512694, -3.504269196027526512 ) ) ;
#844 = AXIS2_PLACEMENT_3D ( 'NONE', #3298, #2542, #6009 ) ;
#845 = CARTESIAN_POINT ( 'NONE',  ( 1.799999999999996048, 0.000000000000000000, -10.20000000000000107 ) ) ;
#846 = FACE_OUTER_BOUND ( 'NONE', #2317, .T. ) ;
#847 = VERTEX_POINT ( 'NONE', #1917 ) ;
#848 = CARTESIAN_POINT ( 'NONE',  ( 4.000000000000000000, 0.8378280264232961239, -3.220590601395640018 ) ) ;
#849 = EDGE_CURVE ( 'NONE', #1411, #5556, #4851, .T. ) ;
#850 = DIRECTION ( 'NONE',  ( 1.000000000000000000, 0.000000000000000000, 0.000000000000000000 ) ) ;
#851 = DIRECTION ( 'NONE',  ( 0.000000000000000000, 0.000000000000000000, -1.000000000000000000 ) ) ;
#852 = CARTESIAN_POINT ( 'NONE',  ( 160.0000000000000000, 0.000000000000000000, -123.0000000000000000 ) ) ;
#853 = VERTEX_POINT ( 'NONE', #4710 ) ;
#854 = PLANE ( 'NONE',  #405 ) ;
#855 = CIRCLE ( 'NONE', #6733, 12.44999999999999929 ) ;
#856 = MANIFOLD_SOLID_BREP ( 'OuterRace', #1716 ) ;
#857 = VECTOR ( 'NONE', #3808, 1000.000000000000000 ) ;
#858 = ORIENTED_EDGE ( 'NONE', *, *, #5162, .T. ) ;
#859 = ORIENTED_EDGE ( 'NONE', *, *, #4888, .F. ) ;
#860 =( REPRESENTATION_RELATIONSHIP ('NONE','NONE', #5587, #5294 ) REPRESENTATION_RELATIONSHIP_WITH_TRANSFORMATION ( #4393 )SHAPE_REPRESENTATION_RELATIONSHIP( ) );
#861 = CARTESIAN_POINT ( 'NONE',  ( 4.000000000000000000, -1.560351142792952617, -0.2242961665059816367 ) ) ;
#862 = CARTESIAN_POINT ( 'NONE',  ( 0.000000000000000000, 0.000000000000000000, 150.0000000000000000 ) ) ;
#863 = CARTESIAN_POINT ( 'NONE',  ( -30.00000000000002842, -20.00000000000000000, 140.0000000000000000 ) ) ;
#864 = CARTESIAN_POINT ( 'NONE',  ( -4.000000000000000000, 0.3987449864459974846, -0.01220643443059782861 ) ) ;
#865 = ADVANCED_FACE ( 'NONE', ( #4376 ), #2371, .F. ) ;
#866 = AXIS2_PLACEMENT_3D ( 'NONE', #939, #3814, #4267 ) ;
#867 = DIRECTION ( 'NONE',  ( 0.000000000000000000, 1.000000000000000000, 0.000000000000000000 ) ) ;
#868 = DIRECTION ( 'NONE',  ( 0.000000000000000000, 0.000000000000000000, -1.000000000000000000 ) ) ;
#869 = ORIENTED_EDGE ( 'NONE', *, *, #7028, .F. ) ;
#870 = PRODUCT ( 'angular contact ball bearing_68_iso_ISO 15 ABB - 1720 - 28,SI,NC,28_68', 'angular contact ball bearing_68_iso_ISO 15 ABB - 1720 - 28,SI,NC,28_68', '', ( #4556 ) ) ;
#871 = LINE ( 'NONE', #916, #4310 ) ;
#872 = VECTOR ( 'NONE', #2495, 999.9999999999998863 ) ;
#873 = DIRECTION ( 'NONE',  ( -0.000000000000000000, -0.000000000000000000, 1.000000000000000000 ) ) ;
#874 = AXIS2_PLACEMENT_3D ( 'NONE', #975, #3396, #1611 ) ;
#875 = ORIENTED_EDGE ( 'NONE', *, *, #1964, .T. ) ;
#876 = CARTESIAN_POINT ( 'NONE',  ( 0.000000000000000000, 8.660254037844390851, -140.0000000000000000 ) ) ;
#877 = SURFACE_STYLE_USAGE ( .BOTH. , #6014 ) ;
#878 = ADVANCED_FACE ( 'NONE', ( #5487 ), #4258, .F. ) ;
#879 = CARTESIAN_POINT ( 'NONE',  ( 2.500000000000000000, 2.357898499370433054, -1.951563910473907981E-15 ) ) ;
#880 = AXIS2_PLACEMENT_3D ( 'NONE', #156, #86, #710 ) ;
#881 = ITEM_DEFINED_TRANSFORMATION ( 'NONE', 'NONE', #3990,  #1963 ) ;
#882 = CARTESIAN_POINT ( 'NONE',  ( 386.6666666666666288, -25.00000000000000000, -159.8500000000001080 ) ) ;
#883 = AXIS2_PLACEMENT_3D ( 'NONE', #6871, #1692, #6315 ) ;
#884 = ORIENTED_EDGE ( 'NONE', *, *, #6060, .F. ) ;
#885 = CARTESIAN_POINT ( 'NONE',  ( 360.0000000000000000, 0.000000000000000000, 0.000000000000000000 ) ) ;
#886 = ORIENTED_EDGE ( 'NONE', *, *, #956, .T. ) ;
#887 = TOROIDAL_SURFACE ( 'NONE', #3398, 10.20000000000000107, 0.2000000000000031197 ) ;
#888 = PLANE ( 'NONE',  #6650 ) ;
#889 = CARTESIAN_POINT ( 'NONE',  ( -20.63749999999999574, 0.000000000000000000, 0.000000000000000000 ) ) ;
#890 = DIRECTION ( 'NONE',  ( -0.000000000000000000, -0.000000000000000000, -1.000000000000000000 ) ) ;
#891 = CIRCLE ( 'NONE', #4830, 2.649999999999985700 ) ;
#892 = ORIENTED_EDGE ( 'NONE', *, *, #728, .F. ) ;
#893 = AXIS2_PLACEMENT_3D ( 'NONE', #5024, #2004, #2641 ) ;
#894 = CARTESIAN_POINT ( 'NONE',  ( 470.0000000000000000, -20.00000000000000000, 200.0000000000000000 ) ) ;
#895 = ITEM_DEFINED_TRANSFORMATION ( 'NONE', 'NONE', #1351,  #1963 ) ;
#896 = FACE_OUTER_BOUND ( 'NONE', #1807, .T. ) ;
#897 = LINE ( 'NONE', #936, #3507 ) ;
#898 = AXIS2_PLACEMENT_3D ( 'NONE', #964, #929, #5484 ) ;
#899 = CARTESIAN_POINT ( 'NONE',  ( 53.33333333333330017, -10.00000000000000000, 162.5000000000000853 ) ) ;
#900 = ORIENTED_EDGE ( 'NONE', *, *, #6139, .F. ) ;
#901 = CARTESIAN_POINT ( 'NONE',  ( 10.00000000000000000, 1.224646799147353256E-15, 140.0000000000000000 ) ) ;
#902 = ADVANCED_FACE ( 'NONE', ( #7143 ), #5410, .F. ) ;
#903 = EDGE_LOOP ( 'NONE', ( #1637, #4277, #2481, #4578 ) ) ;
#904 = EDGE_LOOP ( 'NONE', ( #3846, #3143, #3187, #4503 ) ) ;
#905 = CARTESIAN_POINT ( 'NONE',  ( 53.33333333333330017, -14.99999999999999822, 159.8500000000001080 ) ) ;
#906 = VECTOR ( 'NONE', #6488, 1000.000000000000000 ) ;
#907 = PLANE ( 'NONE',  #5104 ) ;
#908 = DIRECTION ( 'NONE',  ( -0.7071067811865306973, 0.000000000000000000, 0.7071067811865643371 ) ) ;
#909 = LINE ( 'NONE', #5430, #6286 ) ;
#910 = CARTESIAN_POINT ( 'NONE',  ( 53.33333333333330017, -15.00000000000000000, 165.1500000000000625 ) ) ;
#911 = DIRECTION ( 'NONE',  ( -0.000000000000000000, 1.000000000000000000, -0.000000000000000000 ) ) ;
#912 = DIRECTION ( 'NONE',  ( 0.000000000000000000, 0.000000000000000000, -1.000000000000000000 ) ) ;
#913 = VECTOR ( 'NONE', #5806, 1000.000000000000000 ) ;
#914 = ORIENTED_EDGE ( 'NONE', *, *, #920, .T. ) ;
#915 = ADVANCED_FACE ( 'NONE', ( #846 ), #6580, .F. ) ;
#916 = CARTESIAN_POINT ( 'NONE',  ( 13.50000000000000000, 1.653273178848926867E-15, -121.0000000000000000 ) ) ;
#917 = DIRECTION ( 'NONE',  ( 0.000000000000000000, 0.000000000000000000, -1.000000000000000000 ) ) ;
#918 = VERTEX_POINT ( 'NONE', #1997 ) ;
#919 = DIRECTION ( 'NONE',  ( 1.000000000000000000, 0.000000000000000000, -0.000000000000000000 ) ) ;
#920 = EDGE_CURVE ( 'NONE', #1078, #2826, #2516, .T. ) ;
#921 = AXIS2_PLACEMENT_3D ( 'NONE', #299, #2557, #3103 ) ;
#922 = B_SPLINE_CURVE_WITH_KNOTS ( 'NONE', 3,
 ( #3169, #356, #3590, #2467, #804, #3058 ),
 .UNSPECIFIED., .F., .F.,
 ( 4, 2, 4 ),
 ( 0.000000000000000000, 0.0002095117440854740156, 0.0004190234881709480313 ),
 .UNSPECIFIED. ) ;
#923 = CARTESIAN_POINT ( 'NONE',  ( -2.000000000000001776, 1.564486285910744042E-15, 12.77500000000000213 ) ) ;
#924 = LINE ( 'NONE', #7256, #3423 ) ;
#925 = ORIENTED_EDGE ( 'NONE', *, *, #2603, .F. ) ;
#926 = EDGE_CURVE ( 'NONE', #5946, #2821, #3721, .T. ) ;
#927 = CARTESIAN_POINT ( 'NONE',  ( 240.0000000000000000, 0.000000000000000000, 123.0000000000000000 ) ) ;
#928 = ORIENTED_EDGE ( 'NONE', *, *, #2272, .F. ) ;
#929 = DIRECTION ( 'NONE',  ( 0.000000000000000000, 1.000000000000000000, 0.000000000000000000 ) ) ;
#930 = CARTESIAN_POINT ( 'NONE',  ( -4.154094228333456762, 2.398367420968013253, -3.721909803043220055 ) ) ;
#931 = SURFACE_SIDE_STYLE ('',( #3074 ) ) ;
#932 = VERTEX_POINT ( 'NONE', #6625 ) ;
#933 = CARTESIAN_POINT ( 'NONE',  ( 2.500000000000000000, -1.178949249685218303, -2.041999999999998039 ) ) ;
#934 = FACE_OUTER_BOUND ( 'NONE', #4798, .T. ) ;
#935 = DIRECTION ( 'NONE',  ( 0.000000000000000000, 0.000000000000000000, -1.000000000000000000 ) ) ;
#936 = CARTESIAN_POINT ( 'NONE',  ( 325.0000000000000000, 8.660254037844390851, 145.0000000000000284 ) ) ;
#937 = DIRECTION ( 'NONE',  ( 6.123233995736766036E-17, -1.000000000000000000, 0.000000000000000000 ) ) ;
#938 = ORIENTED_EDGE ( 'NONE', *, *, #6072, .T. ) ;
#939 = CARTESIAN_POINT ( 'NONE',  ( 0.000000000000000000, 0.000000000000000000, 125.0000000000000000 ) ) ;
#940 = PRODUCT_DEFINITION_SHAPE ( 'NONE', 'NONE',  #1667 ) ;
#941 = EDGE_CURVE ( 'NONE', #5766, #918, #1514, .T. ) ;
#942 = ORIENTED_EDGE ( 'NONE', *, *, #5085, .T. ) ;
#943 = EDGE_LOOP ( 'NONE', ( #7044, #3226 ) ) ;
#944 = CARTESIAN_POINT ( 'NONE',  ( 4.999999999999999112, 8.660254037844390851, 150.0000000000000000 ) ) ;
#945 = CARTESIAN_POINT ( 'NONE',  ( -5.000000000000000888, -8.660254037844389075, 145.0000000000000284 ) ) ;
#946 = CARTESIAN_POINT ( 'NONE',  ( 2.171643655288379993, -3.365003104552334978, -1.195831703456429434E-14 ) ) ;
#947 = CARTESIAN_POINT ( 'NONE',  ( 365.0000000000000000, 8.660254037844390851, 139.9990000000000236 ) ) ;
#948 = EDGE_CURVE ( 'NONE', #4387, #2711, #5451, .T. ) ;
#949 = CARTESIAN_POINT ( 'NONE',  ( 0.7826237921249276086, 1.524685264938454646E-15, -12.44999999999999929 ) ) ;
#950 = DIRECTION ( 'NONE',  ( 0.000000000000000000, 0.000000000000000000, -1.000000000000000000 ) ) ;
#951 = SHAPE_REPRESENTATION ( 'socket head cap screw_iso_ISO 4762 M5 x 20 - 20N', ( #1963 ), #4003 ) ;
#952 = ORIENTED_EDGE ( 'NONE', *, *, #1964, .F. ) ;
#953 = CARTESIAN_POINT ( 'NONE',  ( 195.0000000000000000, 8.660254037844390851, 145.0000000000000284 ) ) ;
#954 = DIRECTION ( 'NONE',  ( 0.000000000000000000, -1.000000000000000000, 0.000000000000000000 ) ) ;
#955 = DIRECTION ( 'NONE',  ( -0.000000000000000000, 1.000000000000000000, -0.000000000000000000 ) ) ;
#956 = EDGE_CURVE ( 'NONE', #6406, #3386, #3684, .T. ) ;
#957 = FILL_AREA_STYLE_COLOUR ( '', #5782 ) ;
#958 = EDGE_CURVE ( 'NONE', #7221, #4390, #202, .T. ) ;
#959 = DIRECTION ( 'NONE',  ( 1.000000000000000000, 0.000000000000000000, 0.000000000000000000 ) ) ;
#960 = ORIENTED_EDGE ( 'NONE', *, *, #4756, .F. ) ;
#961 = ORIENTED_EDGE ( 'NONE', *, *, #6276, .T. ) ;
#962 = DIRECTION ( 'NONE',  ( 1.000000000000000000, 0.000000000000000000, 0.000000000000000000 ) ) ;
#963 = EDGE_LOOP ( 'NONE', ( #3170, #5909, #4292, #1829 ) ) ;
#964 = CARTESIAN_POINT ( 'NONE',  ( 136.6666666666666288, -20.00000000000000000, 162.5000000000000853 ) ) ;
#965 = VECTOR ( 'NONE', #5168, 1000.000000000000000 ) ;
#966 = ADVANCED_FACE ( 'NONE', ( #6106 ), #1749, .T. ) ;
#967 = DIRECTION ( 'NONE',  ( 1.000000000000000000, 0.000000000000000000, 0.000000000000000000 ) ) ;
#968 = CARTESIAN_POINT ( 'NONE',  ( 0.000000000000000000, 0.000000000000000000, -4.000000000000000000 ) ) ;
#969 = ORIENTED_EDGE ( 'NONE', *, *, #234, .T. ) ;
#970 = VECTOR ( 'NONE', #3753, 1000.000000000000000 ) ;
#971 = FACE_OUTER_BOUND ( 'NONE', #6440, .T. ) ;
#972 = CONTEXT_DEPENDENT_SHAPE_REPRESENTATION ( #6373, #2270 ) ;
#973 = PLANE ( 'NONE',  #6249 ) ;
#974 = FACE_BOUND ( 'NONE', #903, .T. ) ;
#975 = CARTESIAN_POINT ( 'NONE',  ( 120.0000000000000000, 0.000000000000000000, 0.000000000000000000 ) ) ;
#976 = EDGE_CURVE ( 'NONE', #1043, #7189, #7265, .T. ) ;
#977 = VERTEX_POINT ( 'NONE', #1566 ) ;
#978 = CARTESIAN_POINT ( 'NONE',  ( 3.333333333333335702, -2.694301256218268215, -3.300726591567084256 ) ) ;
#979 = AXIS2_PLACEMENT_3D ( 'NONE', #799, #3053, #4229 ) ;
#980 = EDGE_LOOP ( 'NONE', ( #1441, #2729, #2992, #5121 ) ) ;
#981 = ORIENTED_EDGE ( 'NONE', *, *, #1995, .F. ) ;
#982 = FACE_OUTER_BOUND ( 'NONE', #1058, .T. ) ;
#983 = CARTESIAN_POINT ( 'NONE',  ( -1.800000000000002931, 0.000000000000000000, 0.000000000000000000 ) ) ;
#984 = ITEM_DEFINED_TRANSFORMATION ( 'NONE', 'NONE', #3140,  #1963 ) ;
#985 = LINE ( 'NONE', #2099, #3236 ) ;
#986 = DIRECTION ( 'NONE',  ( -1.000000000000000000, -0.000000000000000000, -0.000000000000000000 ) ) ;
#987 = VECTOR ( 'NONE', #815, 1000.000000000000000 ) ;
#988 = DIRECTION ( 'NONE',  ( 1.000000000000000000, 0.000000000000000000, -0.000000000000000000 ) ) ;
#989 = PRODUCT_DEFINITION_CONTEXT ( 'detailed design', #5793, 'design' ) ;
#990 = LINE ( 'NONE', #3293, #3256 ) ;
#991 = EDGE_LOOP ( 'NONE', ( #5668, #2360, #2719, #1798 ) ) ;
#992 = AXIS2_PLACEMENT_3D ( 'NONE', #1897, #6975, #4193 ) ;
#993 = DIRECTION ( 'NONE',  ( 0.000000000000000000, 0.000000000000000000, 1.000000000000000000 ) ) ;
#994 = CARTESIAN_POINT ( 'NONE',  ( 114.9999999999999858, 8.660254037844390851, 140.0000000000000000 ) ) ;
#995 = CARTESIAN_POINT ( 'NONE',  ( -0.6448876103708541807, -4.246476118072358474, -0.2256878752776773356 ) ) ;
#996 = CARTESIAN_POINT ( 'NONE',  ( 219.9999999999999716, -20.00000000000000000, 162.5000000000000853 ) ) ;
#997 = APPLICATION_PROTOCOL_DEFINITION ( 'draft international standard', 'automotive_design', 1998, #3877 ) ;
#998 =( BOUNDED_SURFACE ( )  B_SPLINE_SURFACE ( 3, 2, ( 
 ( #5283, #2322, #5148 ),
 ( #1736, #3415, #1243 ),
 ( #2943, #6915, #4729 ),
 ( #4050, #1281, #3984 ),
 ( #166, #1832, #4025 ),
 ( #7018, #6939, #722 ) ),
 .UNSPECIFIED., .F., .F., .T. ) 
 B_SPLINE_SURFACE_WITH_KNOTS ( ( 4, 2, 4 ),
 ( 3, 3 ),
 ( 0.02032853247518125531, 0.02278863295364820865, 0.02524873343211516200 ),
 ( 0.000000000000000000, 1.000000000000000000 ),
 .UNSPECIFIED. ) 
 GEOMETRIC_REPRESENTATION_ITEM ( )  RATIONAL_B_SPLINE_SURFACE ( (
 ( 1.000000000000000000, 0.8047781615896836271, 1.000000000000000000),
 ( 1.000000000000000000, 0.8123767586289967202, 1.000000000000000000),
 ( 1.000000000000000000, 0.8190662415563443322, 1.000000000000000000),
 ( 1.000000000000000000, 0.8192361015669982205, 1.000000000000000000),
 ( 1.000000000000000000, 0.8126135807103181952, 1.000000000000000000),
 ( 1.000000000000000000, 0.8047712338318587788, 1.000000000000000000) ) ) 
 REPRESENTATION_ITEM ( '' )  SURFACE ( )  );
#999 = DIRECTION ( 'NONE',  ( -0.000000000000000000, -0.000000000000000000, 1.000000000000000000 ) ) ;
#1000 = VERTEX_POINT ( 'NONE', #3845 ) ;
#1001 = ORIENTED_EDGE ( 'NONE', *, *, #3815, .T. ) ;
#1002 = EDGE_CURVE ( 'NONE', #719, #853, #6743, .T. ) ;
#1003 = DIRECTION ( 'NONE',  ( 1.000000000000000000, 0.000000000000000000, 0.000000000000000000 ) ) ;
#1004 = VERTEX_POINT ( 'NONE', #5611 ) ;
#1005 = FACE_OUTER_BOUND ( 'NONE', #5871, .T. ) ;
#1006 = AXIS2_PLACEMENT_3D ( 'NONE', #5789, #3994, #3452 ) ;
#1007 = VECTOR ( 'NONE', #5328, 1000.000000000000000 ) ;
#1008 = AXIS2_PLACEMENT_3D ( 'NONE', #4801, #1517, #3094 ) ;
#1009 = CYLINDRICAL_SURFACE ( 'NONE', #5553, 2.649999999999985700 ) ;
#1010 = CARTESIAN_POINT ( 'NONE',  ( 136.6666666666666288, -25.00000000000000000, 162.5000000000000853 ) ) ;
#1011 = ORIENTED_EDGE ( 'NONE', *, *, #5466, .T. ) ;
#1012 = VECTOR ( 'NONE', #620, 1000.000000000000114 ) ;
#1013 = CONICAL_SURFACE ( 'NONE', #1245, 5.560781378645573980, 1.221730476396046816 ) ;
#1014 = EDGE_CURVE ( 'NONE', #5089, #5864, #453, .T. ) ;
#1015 = FACE_BOUND ( 'NONE', #4450, .T. ) ;
#1016 = LINE ( 'NONE', #3155, #2036 ) ;
#1017 = DIRECTION ( 'NONE',  ( -0.000000000000000000, -0.000000000000000000, 1.000000000000000000 ) ) ;
#1018 = EDGE_CURVE ( 'NONE', #1043, #3333, #7260, .T. ) ;
#1019 = DIRECTION ( 'NONE',  ( 1.000000000000000000, 0.000000000000000000, 0.000000000000000000 ) ) ;
#1020 =( REPRESENTATION_RELATIONSHIP ('NONE','NONE', #5587, #951 ) REPRESENTATION_RELATIONSHIP_WITH_TRANSFORMATION ( #138 )SHAPE_REPRESENTATION_RELATIONSHIP( ) );
#1021 = EDGE_LOOP ( 'NONE', ( #1633, #1670, #6133, #3807 ) ) ;
#1022 = CIRCLE ( 'NONE', #661, 11.00000000000000000 ) ;
#1023 = CARTESIAN_POINT ( 'NONE',  ( 45.00000000000000000, 8.660254037844390851, 139.9990000000000236 ) ) ;
#1024 = ORIENTED_EDGE ( 'NONE', *, *, #3658, .F. ) ;
#1025 = ORIENTED_EDGE ( 'NONE', *, *, #5063, .F. ) ;
#1026 = EDGE_CURVE ( 'NONE', #271, #6816, #6904, .T. ) ;
#1027 = PLANE ( 'NONE',  #4902 ) ;
#1028 = CARTESIAN_POINT ( 'NONE',  ( 1.274258131564866448, 3.883108878240963513, -3.220599429844046568 ) ) ;
#1029 = CIRCLE ( 'NONE', #780, 19.00000000000000000 ) ;
#1030 = LINE ( 'NONE', #3289, #2044 ) ;
#1031 = CARTESIAN_POINT ( 'NONE',  ( 2.500000000000000000, 1.178949249685213863, -2.042000000000001148 ) ) ;
#1032 = DIRECTION ( 'NONE',  ( 1.000000000000000000, 0.000000000000000000, 0.000000000000000000 ) ) ;
#1033 = FACE_OUTER_BOUND ( 'NONE', #3956, .T. ) ;
#1034 = VECTOR ( 'NONE', #5723, 1000.000000000000000 ) ;
#1035 = ORIENTED_EDGE ( 'NONE', *, *, #7145, .F. ) ;
#1036 = CIRCLE ( 'NONE', #1847, 2.649999999999985700 ) ;
#1037 = CARTESIAN_POINT ( 'NONE',  ( 4.000000000000000000, 2.309401076758515803, -0.4999999999999995559 ) ) ;
#1038 = FACE_BOUND ( 'NONE', #5519, .T. ) ;
#1039 = LINE ( 'NONE', #2109, #7181 ) ;
#1040 = DIRECTION ( 'NONE',  ( -1.000000000000000000, 0.000000000000000000, 0.000000000000000000 ) ) ;
#1041 = VECTOR ( 'NONE', #157, 1000.000000000000000 ) ;
#1042 = CARTESIAN_POINT ( 'NONE',  ( 2.548804901056335857E-15, 4.736522675502163437, -3.681124513963624612 ) ) ;
#1043 = VERTEX_POINT ( 'NONE', #2156 ) ;
#1044 = ORIENTED_EDGE ( 'NONE', *, *, #286, .F. ) ;
#1046 = AXIS2_PLACEMENT_3D ( 'NONE', #5157, #5053, #4000 ) ;
#1045 = DIRECTION ( 'NONE',  ( 1.000000000000000000, 0.000000000000000000, 0.000000000000000000 ) ) ;
#1047 = ORIENTED_EDGE ( 'NONE', *, *, #5906, .F. ) ;
#1048 = LINE ( 'NONE', #7298, #4130 ) ;
#1049 = EDGE_CURVE ( 'NONE', #6322, #1596, #6310, .T. ) ;
#1050 = DIRECTION ( 'NONE',  ( 0.000000000000000000, 0.000000000000000000, 1.000000000000000000 ) ) ;
#1051 = CARTESIAN_POINT ( 'NONE',  ( 4.999999999999999112, 8.660254037844390851, -150.0000000000000000 ) ) ;
#1052 = ORIENTED_EDGE ( 'NONE', *, *, #819, .T. ) ;
#1053 = MECHANICAL_DESIGN_GEOMETRIC_PRESENTATION_REPRESENTATION (  '', ( #6545 ), #1983 ) ;
#1054 = DIRECTION ( 'NONE',  ( 0.000000000000000000, -0.000000000000000000, 1.000000000000000000 ) ) ;
#1055 = ITEM_DEFINED_TRANSFORMATION ( 'NONE', 'NONE', #1006,  #1963 ) ;
#1056 = DIRECTION ( 'NONE',  ( -0.000000000000000000, 1.000000000000000000, -0.000000000000000000 ) ) ;
#1057 = CARTESIAN_POINT ( 'NONE',  ( 80.00000000000000000, 0.000000000000000000, 123.0000000000000000 ) ) ;
#1058 = EDGE_LOOP ( 'NONE', ( #4774, #6983, #2551, #626 ) ) ;
#1059 = DIRECTION ( 'NONE',  ( 0.000000000000000000, 0.000000000000000000, -1.000000000000000000 ) ) ;
#1060 = EDGE_CURVE ( 'NONE', #6894, #5855, #4448, .T. ) ;
#1061 = ORIENTED_EDGE ( 'NONE', *, *, #5857, .T. ) ;
#1062 = ORIENTED_EDGE ( 'NONE', *, *, #6098, .T. ) ;
#1063 = DIRECTION ( 'NONE',  ( 1.000000000000000000, 0.000000000000000000, -0.000000000000000000 ) ) ;
#1064 = CARTESIAN_POINT ( 'NONE',  ( 1.287237434362044075, 3.875615274277557809, -3.430618716626812059 ) ) ;
#1065 = CARTESIAN_POINT ( 'NONE',  ( -0.2277608394786177770, 0.000000000000000000, 12.77499999999999858 ) ) ;
#1066 = CARTESIAN_POINT ( 'NONE',  ( 5.000000000000002665, 0.000000000000000000, -2.700000000000001066 ) ) ;
#1067 = LINE ( 'NONE', #2613, #3000 ) ;
#1068 = DIRECTION ( 'NONE',  ( -1.000000000000000000, 0.000000000000000000, 0.000000000000000000 ) ) ;
#1069 = CYLINDRICAL_SURFACE ( 'NONE', #764, 19.00000000000000000 ) ;
#1070 = EDGE_CURVE ( 'NONE', #6814, #1780, #4561, .T. ) ;
#1071 = ORIENTED_EDGE ( 'NONE', *, *, #778, .F. ) ;
#1072 = DIRECTION ( 'NONE',  ( -0.000000000000000000, -0.000000000000000000, 1.000000000000000000 ) ) ;
#1073 = EDGE_CURVE ( 'NONE', #7081, #5227, #4988, .T. ) ;
#1074 = DIRECTION ( 'NONE',  ( 0.000000000000000000, -1.000000000000000000, 0.000000000000000000 ) ) ;
#1075 = CARTESIAN_POINT ( 'NONE',  ( 35.00000000000000000, -8.660254037844389075, 139.9990000000000236 ) ) ;
#1076 = CYLINDRICAL_SURFACE ( 'NONE', #4002, 2.649999999999985700 ) ;
#1077 = ORIENTED_EDGE ( 'NONE', *, *, #2199, .F. ) ;
#1078 = VERTEX_POINT ( 'NONE', #3427 ) ;
#1079 = CONTEXT_DEPENDENT_SHAPE_REPRESENTATION ( #449, #4212 ) ;
#1080 = ORIENTED_EDGE ( 'NONE', *, *, #7028, .T. ) ;
#1081 = DIRECTION ( 'NONE',  ( 0.000000000000000000, -1.000000000000000000, 0.000000000000000000 ) ) ;
#1082 = PRODUCT_RELATED_PRODUCT_CATEGORY ( 'part', '', ( #4278 ) ) ;
#1083 = CARTESIAN_POINT ( 'NONE',  ( 4.999999999999999112, 0.000000000000000000, 140.0000000000000000 ) ) ;
#1084 = VERTEX_POINT ( 'NONE', #3312 ) ;
#1085 = LINE ( 'NONE', #2985, #6754 ) ;
#1086 = PLANE ( 'NONE',  #3101 ) ;
#1087 = LINE ( 'NONE', #2161, #5433 ) ;
#1088 = AXIS2_PLACEMENT_3D ( 'NONE', #3698, #5427, #3116 ) ;
#1089 = CARTESIAN_POINT ( 'NONE',  ( 160.0000000000000000, 0.000000000000000000, 0.000000000000000000 ) ) ;
#1090 = ORIENTED_EDGE ( 'NONE', *, *, #288, .F. ) ;
#1091 = PLANE ( 'NONE',  #6280 ) ;
#1092 = AXIS2_PLACEMENT_3D ( 'NONE', #1591, #4402, #6129 ) ;
#1093 = ORIENTED_EDGE ( 'NONE', *, *, #5913, .F. ) ;
#1094 = EDGE_CURVE ( 'NONE', #6847, #3802, #5018, .T. ) ;
#1095 = ORIENTED_EDGE ( 'NONE', *, *, #6194, .T. ) ;
#1096 = CARTESIAN_POINT ( 'NONE',  ( -0.1756481739660520902, 4.720212674038980261, -3.469390959564065291 ) ) ;
#1097 = LINE ( 'NONE', #3327, #6852 ) ;
#1098 = DIRECTION ( 'NONE',  ( 1.000000000000000000, 0.000000000000000000, -0.000000000000000000 ) ) ;
#1099 = VECTOR ( 'NONE', #2386, 1000.000000000000000 ) ;
#1100 = ORIENTED_EDGE ( 'NONE', *, *, #6031, .T. ) ;
#1101 = FACE_OUTER_BOUND ( 'NONE', #7030, .T. ) ;
#1102 = ORIENTED_EDGE ( 'NONE', *, *, #4356, .T. ) ;
#1103 = DIRECTION ( 'NONE',  ( 0.000000000000000000, -0.000000000000000000, -1.000000000000000000 ) ) ;
#1104 = CARTESIAN_POINT ( 'NONE',  ( 2.500000000000000000, 0.000000000000000000, 0.000000000000000000 ) ) ;
#1105 = CARTESIAN_POINT ( 'NONE',  ( 2.500000000000000000, 2.500728763858895382E-16, -2.041999999999999815 ) ) ;
#1106 =( NAMED_UNIT ( * ) PLANE_ANGLE_UNIT ( ) SI_UNIT ( $, .RADIAN. ) );
#1107 = ADVANCED_FACE ( 'NONE', ( #5095 ), #3964, .F. ) ;
#1108 = CIRCLE ( 'NONE', #4667, 2.100000000000000089 ) ;
#1109 = AXIS2_PLACEMENT_3D ( 'NONE', #6519, #7075, #1923 ) ;
#1110 = ORIENTED_EDGE ( 'NONE', *, *, #1503, .F. ) ;
#1111 = VERTEX_POINT ( 'NONE', #3887 ) ;
#1112 = VECTOR ( 'NONE', #5415, 1000.000000000000000 ) ;
#1113 = APPLICATION_PROTOCOL_DEFINITION ( 'draft international standard', 'automotive_design', 1998, #5129 ) ;
#1114 = ORIENTED_EDGE ( 'NONE', *, *, #6818, .F. ) ;
#1115 = EDGE_CURVE ( 'NONE', #3386, #84, #6853, .T. ) ;
#1116 = DIRECTION ( 'NONE',  ( 0.000000000000000000, 1.000000000000000000, 0.000000000000000000 ) ) ;
#1117 = AXIS2_PLACEMENT_3D ( 'NONE', #1452, #308, #1420 ) ;
#1118 = CARTESIAN_POINT ( 'NONE',  ( 470.0000000000000000, -15.00000000000000000, 180.0000000000000284 ) ) ;
#1119 = ORIENTED_EDGE ( 'NONE', *, *, #5813, .F. ) ;
#1120 = DIRECTION ( 'NONE',  ( 0.000000000000000000, 0.000000000000000000, 1.000000000000000000 ) ) ;
#1121 = FACE_BOUND ( 'NONE', #5959, .T. ) ;
#1122 = CIRCLE ( 'NONE', #2298, 12.44999999999999929 ) ;
#1123 = AXIS2_PLACEMENT_3D ( 'NONE', #5161, #1127, #4499 ) ;
#1124 = LINE ( 'NONE', #2758, #4238 ) ;
#1125 = AXIS2_PLACEMENT_3D ( 'NONE', #1511, #4353, #5626 ) ;
#1126 = AXIS2_PLACEMENT_3D ( 'NONE', #4658, #5647, #5099 ) ;
#1127 = DIRECTION ( 'NONE',  ( 6.123233995736766036E-17, -1.000000000000000000, 0.000000000000000000 ) ) ;
#1128 = ORIENTED_EDGE ( 'NONE', *, *, #1710, .T. ) ;
#1129 = FACE_OUTER_BOUND ( 'NONE', #1317, .T. ) ;
#1130 = AXIS2_PLACEMENT_3D ( 'NONE', #6354, #2924, #108 ) ;
#1131 = AXIS2_PLACEMENT_3D ( 'NONE', #6762, #7281, #1465 ) ;
#1132 = ORIENTED_EDGE ( 'NONE', *, *, #7005, .F. ) ;
#1133 = CARTESIAN_POINT ( 'NONE',  ( 0.000000000000000000, 0.000000000000000000, 121.0000000000000000 ) ) ;
#1134 = DIRECTION ( 'NONE',  ( 0.000000000000000000, 1.000000000000000000, 0.000000000000000000 ) ) ;
#1135 = DIRECTION ( 'NONE',  ( 0.000000000000000000, 0.000000000000000000, 1.000000000000000000 ) ) ;
#1136 = DIRECTION ( 'NONE',  ( 0.000000000000000000, 0.000000000000000000, 1.000000000000000000 ) ) ;
#1137 = CIRCLE ( 'NONE', #6395, 2.649999999999985700 ) ;
#1138 = VECTOR ( 'NONE', #1649, 1000.000000000000000 ) ;
#1139 = ORIENTED_EDGE ( 'NONE', *, *, #3973, .T. ) ;
#1140 = DIRECTION ( 'NONE',  ( -0.000000000000000000, -0.000000000000000000, 1.000000000000000000 ) ) ;
#1141 = EDGE_CURVE ( 'NONE', #4157, #630, #4032, .T. ) ;
#1142 = VERTEX_POINT ( 'NONE', #1707 ) ;
#1143 = VECTOR ( 'NONE', #545, 1000.000000000000000 ) ;
#1144 = COLOUR_RGB ( '',1.000000000000000000, 0.9490196078431372140, 0.9098039215686274384 ) ;
#1145 = CARTESIAN_POINT ( 'NONE',  ( -2.688821387764050996E-14, -4.618802153517012954, -0.4999999999999995559 ) ) ;
#1146 = CARTESIAN_POINT ( 'NONE',  ( 2.500000000000000000, 2.357898499370433054, -1.951563910473907981E-15 ) ) ;
#1147 = CYLINDRICAL_SURFACE ( 'NONE', #2971, 2.649999999999985700 ) ;
#1148 = LINE ( 'NONE', #3417, #4961 ) ;
#1149 = CIRCLE ( 'NONE', #439, 5.560781378645573980 ) ;
#1150 = CARTESIAN_POINT ( 'NONE',  ( -4.000000000000000000, 2.309401076758498483, -3.433295621305379353 ) ) ;
#1151 = EDGE_CURVE ( 'NONE', #2749, #1904, #6663, .T. ) ;
#1152 = ORIENTED_EDGE ( 'NONE', *, *, #3553, .F. ) ;
#1153 = EDGE_CURVE ( 'NONE', #932, #266, #492, .T. ) ;
#1154 = ITEM_DEFINED_TRANSFORMATION ( 'NONE', 'NONE', #6622,  #1963 ) ;
#1155 = EDGE_LOOP ( 'NONE', ( #3247, #2570 ) ) ;
#1156 = PRODUCT_DEFINITION_SHAPE ( 'NONE', 'NONE',  #7411 ) ;
#1157 = DIRECTION ( 'NONE',  ( -1.000000000000000000, 0.000000000000000000, -0.000000000000000000 ) ) ;
#1158 = DIRECTION ( 'NONE',  ( -0.000000000000000000, 1.000000000000000000, -0.000000000000000000 ) ) ;
#1159 = EDGE_CURVE ( 'NONE', #1397, #2205, #2191, .T. ) ;
#1160 = AXIS2_PLACEMENT_3D ( 'NONE', #2718, #526, #4490 ) ;
#1161 = EDGE_LOOP ( 'NONE', ( #6055, #3583, #7024, #1945 ) ) ;
#1162 =( REPRESENTATION_RELATIONSHIP ('NONE','NONE', #5587, #5294 ) REPRESENTATION_RELATIONSHIP_WITH_TRANSFORMATION ( #5548 )SHAPE_REPRESENTATION_RELATIONSHIP( ) );
#1163 = DIRECTION ( 'NONE',  ( 0.000000000000000000, 1.000000000000000000, 0.000000000000000000 ) ) ;
#1164 = EDGE_CURVE ( 'NONE', #5386, #5253, #2926, .T. ) ;
#1165 = DIRECTION ( 'NONE',  ( -0.000000000000000000, -0.000000000000000000, 1.000000000000000000 ) ) ;
#1166 = VECTOR ( 'NONE', #250, 1000.000000000000000 ) ;
#1167 = CARTESIAN_POINT ( 'NONE',  ( 200.0000000000000000, 0.000000000000000000, 0.000000000000000000 ) ) ;
#1168 = VERTEX_POINT ( 'NONE', #1118 ) ;
#1169 = DIRECTION ( 'NONE',  ( 0.000000000000000000, 0.000000000000000000, -1.000000000000000000 ) ) ;
#1170 = ORIENTED_EDGE ( 'NONE', *, *, #2359, .T. ) ;
#1171 = CARTESIAN_POINT ( 'NONE',  ( 0.000000000000000000, 0.000000000000000000, -5.000000000000000000 ) ) ;
#1172 = CARTESIAN_POINT ( 'NONE',  ( 0.000000000000000000, 0.000000000000000000, -4.974599999999998801 ) ) ;
#1173 = CONTEXT_DEPENDENT_SHAPE_REPRESENTATION ( #1720, #3462 ) ;
#1174 = DIRECTION ( 'NONE',  ( -0.000000000000000000, 1.000000000000000000, -0.000000000000000000 ) ) ;
#1175 = CARTESIAN_POINT ( 'NONE',  ( 164.9999999999999716, 8.660254037844390851, 139.9990000000000236 ) ) ;
#1176 = EDGE_CURVE ( 'NONE', #1728, #7233, #2230, .T. ) ;
#1177 = ORIENTED_EDGE ( 'NONE', *, *, #6890, .F. ) ;
#1178 = CARTESIAN_POINT ( 'NONE',  ( -5.000000000000000888, 8.660254037844390851, 150.0000000000000000 ) ) ;
#1179 = VERTEX_POINT ( 'NONE', #4139 ) ;
#1180 = DIRECTION ( 'NONE',  ( 0.000000000000000000, 0.000000000000000000, 1.000000000000000000 ) ) ;
#1181 = DIRECTION ( 'NONE',  ( 0.000000000000000000, 1.000000000000000000, 0.000000000000000000 ) ) ;
#1182 = LINE ( 'NONE', #1105, #6356 ) ;
#1183 = CARTESIAN_POINT ( 'NONE',  ( 2.500000000000000000, -2.357898499370432610, 3.252606517456513302E-15 ) ) ;
#1184 = DIRECTION ( 'NONE',  ( 1.000000000000000000, 0.000000000000000000, 0.000000000000000000 ) ) ;
#1185 = ORIENTED_EDGE ( 'NONE', *, *, #3609, .F. ) ;
#1186 = ORIENTED_EDGE ( 'NONE', *, *, #2822, .T. ) ;
#1187 = SHAPE_DEFINITION_REPRESENTATION ( #345, #5294 ) ;
#1188 = ORIENTED_EDGE ( 'NONE', *, *, #5813, .T. ) ;
#1189 = EDGE_CURVE ( 'NONE', #2308, #3238, #6358, .T. ) ;
#1190 =( NAMED_UNIT ( * ) PLANE_ANGLE_UNIT ( ) SI_UNIT ( $, .RADIAN. ) );
#1191 = ADVANCED_FACE ( 'NONE', ( #1775 ), #5192, .F. ) ;
#1192 = CARTESIAN_POINT ( 'NONE',  ( 35.00000000000000000, -8.660254037844389075, 139.9990000000000236 ) ) ;
#1193 = SHAPE_REPRESENTATION ( 'roller axis', ( #1963 ), #5205 ) ;
#1194 = ORIENTED_EDGE ( 'NONE', *, *, #3551, .T. ) ;
#1195 = SURFACE_SIDE_STYLE ('',( #838 ) ) ;
#1196 = CARTESIAN_POINT ( 'NONE',  ( -30.00000000000002842, 15.00000000000000000, 145.0000000000000284 ) ) ;
#1197 = EDGE_CURVE ( 'NONE', #2273, #807, #6922, .T. ) ;
#1198 = ORIENTED_EDGE ( 'NONE', *, *, #5947, .F. ) ;
#1199 = DIRECTION ( 'NONE',  ( 0.000000000000000000, -1.000000000000000000, 0.000000000000000000 ) ) ;
#1200 = APPLICATION_CONTEXT ( 'automotive_design' ) ;
#1201 = ORIENTED_EDGE ( 'NONE', *, *, #4112, .F. ) ;
#1202 = DIRECTION ( 'NONE',  ( 0.000000000000000000, 0.000000000000000000, -1.000000000000000000 ) ) ;
#1203 = DIRECTION ( 'NONE',  ( -0.000000000000000000, -0.000000000000000000, 1.000000000000000000 ) ) ;
#1204 = FACE_OUTER_BOUND ( 'NONE', #2091, .T. ) ;
#1205 = CARTESIAN_POINT ( 'NONE',  ( 395.0000000000000000, 8.660254037844390851, 145.0000000000000284 ) ) ;
#1206 = ADVANCED_FACE ( 'NONE', ( #4742 ), #2925, .F. ) ;
#1207 = VERTEX_POINT ( 'NONE', #703 ) ;
#1208 = LINE ( 'NONE', #1178, #5962 ) ;
#1209 = ORIENTED_EDGE ( 'NONE', *, *, #4502, .F. ) ;
#1210 = LINE ( 'NONE', #3476, #1099 ) ;
#1211 = CARTESIAN_POINT ( 'NONE',  ( 386.6666666666666288, -20.00000000000000000, 162.5000000000000853 ) ) ;
#1212 = VECTOR ( 'NONE', #3174, 1000.000000000000000 ) ;
#1213 = CARTESIAN_POINT ( 'NONE',  ( 315.0000000000000568, 8.660254037844390851, 140.0000000000000000 ) ) ;
#1214 = FACE_BOUND ( 'NONE', #347, .T. ) ;
#1215 = VECTOR ( 'NONE', #6879, 1000.000000000000000 ) ;
#1216 = CARTESIAN_POINT ( 'NONE',  ( 235.0000000000000000, -8.660254037844389075, 145.0000000000000284 ) ) ;
#1217 = ORIENTED_EDGE ( 'NONE', *, *, #7290, .T. ) ;
#1218 = SHAPE_DEFINITION_REPRESENTATION ( #4339, #6025 ) ;
#1219 = ORIENTED_EDGE ( 'NONE', *, *, #1141, .T. ) ;
#1220 = AXIS2_PLACEMENT_3D ( 'NONE', #4115, #2935, #3077 ) ;
#1221 = LINE ( 'NONE', #5794, #210 ) ;
#1222 = EDGE_CURVE ( 'NONE', #3817, #5003, #74, .T. ) ;
#1223 = VECTOR ( 'NONE', #494, 1000.000000000000000 ) ;
#1224 = ORIENTED_EDGE ( 'NONE', *, *, #4343, .T. ) ;
#1225 = CARTESIAN_POINT ( 'NONE',  ( -2.855764796983342624, 2.970025579236414082, -0.09382832055445475272 ) ) ;
#1226 = CARTESIAN_POINT ( 'NONE',  ( 4.000000000000000000, 2.309401076758497151, -5.000000000000000000 ) ) ;
#1227 = ORIENTED_EDGE ( 'NONE', *, *, #3658, .T. ) ;
#1228 = DIRECTION ( 'NONE',  ( 0.000000000000000000, -0.000000000000000000, 1.000000000000000000 ) ) ;
#1229 = ORIENTED_EDGE ( 'NONE', *, *, #5799, .T. ) ;
#1230 = EDGE_CURVE ( 'NONE', #6875, #584, #3489, .T. ) ;
#1231 = CARTESIAN_POINT ( 'NONE',  ( -1.800000000000001155, 0.000000000000000000, 0.000000000000000000 ) ) ;
#1232 = CARTESIAN_POINT ( 'NONE',  ( 2.500000000000000888, 3.061616997868384127E-16, -4.974599999999998801 ) ) ;
#1233 = CONTEXT_DEPENDENT_SHAPE_REPRESENTATION ( #6994, #6949 ) ;
#1234 = CARTESIAN_POINT ( 'NONE',  ( 3.455068668934414777, -2.624017327439094327, -3.316620875263732504 ) ) ;
#1235 = FACE_OUTER_BOUND ( 'NONE', #5839, .T. ) ;
#1236 = ORIENTED_EDGE ( 'NONE', *, *, #5982, .F. ) ;
#1237 = EDGE_LOOP ( 'NONE', ( #4346, #2604, #5037, #3051 ) ) ;
#1238 = DIRECTION ( 'NONE',  ( -0.000000000000000000, -0.000000000000000000, 1.000000000000000000 ) ) ;
#1239 = CIRCLE ( 'NONE', #5300, 9.999999999999994671 ) ;
#1240 = EDGE_CURVE ( 'NONE', #2491, #4387, #1221, .T. ) ;
#1241 = VERTEX_POINT ( 'NONE', #1259 ) ;
#1242 = LINE ( 'NONE', #3584, #6951 ) ;
#1243 = CARTESIAN_POINT ( 'NONE',  ( -0.6640947660597427138, 4.471078309994878985, -3.602146406945963442 ) ) ;
#1244 = AXIS2_PLACEMENT_3D ( 'NONE', #947, #3203, #2653 ) ;
#1245 = AXIS2_PLACEMENT_3D ( 'NONE', #4355, #5763, #637 ) ;
#1246 = DIRECTION ( 'NONE',  ( -1.000000000000000000, -0.000000000000000000, -0.000000000000000000 ) ) ;
#1247 = FACE_OUTER_BOUND ( 'NONE', #4443, .T. ) ;
#1248 = EDGE_CURVE ( 'NONE', #6406, #1422, #218, .T. ) ;
#1249 = LINE ( 'NONE', #6980, #6621 ) ;
#1250 =( REPRESENTATION_RELATIONSHIP ('NONE','NONE', #5587, #6025 ) REPRESENTATION_RELATIONSHIP_WITH_TRANSFORMATION ( #3154 )SHAPE_REPRESENTATION_RELATIONSHIP( ) );
#1251 = VECTOR ( 'NONE', #1924, 1000.000000000000000 ) ;
#1252 = AXIS2_PLACEMENT_3D ( 'NONE', #2724, #7306, #3233 ) ;
#1253 = ORIENTED_EDGE ( 'NONE', *, *, #3381, .F. ) ;
#1254 = ORIENTED_EDGE ( 'NONE', *, *, #4766, .T. ) ;
#1255 = ITEM_DEFINED_TRANSFORMATION ( 'NONE', 'NONE', #3379,  #1963 ) ;
#1256 = DIRECTION ( 'NONE',  ( -1.000000000000000000, 0.000000000000000000, -0.000000000000000000 ) ) ;
#1257 = ORIENTED_EDGE ( 'NONE', *, *, #6327, .T. ) ;
#1258 = VECTOR ( 'NONE', #3930, 1000.000000000000000 ) ;
#1259 = CARTESIAN_POINT ( 'NONE',  ( -2.000000000000007550, -3.464101615137749945, 0.000000000000000000 ) ) ;
#1260 = VECTOR ( 'NONE', #6294, 1000.000000000000000 ) ;
#1261 = ORIENTED_EDGE ( 'NONE', *, *, #6825, .F. ) ;
#1262 = AXIS2_PLACEMENT_3D ( 'NONE', #2572, #4868, #5324 ) ;
#1263 = EDGE_CURVE ( 'NONE', #4634, #4692, #7317, .T. ) ;
#1264 = DIRECTION ( 'NONE',  ( 1.000000000000000000, 0.000000000000000000, 0.000000000000000000 ) ) ;
#1265 = CARTESIAN_POINT ( 'NONE',  ( 35.00000000000000000, 8.660254037844390851, 139.9990000000000236 ) ) ;
#1266 = PRODUCT_DEFINITION_SHAPE ( 'NONE', 'NONE',  #7392 ) ;
#1267 = DIRECTION ( 'NONE',  ( -0.000000000000000000, 1.000000000000000000, -0.000000000000000000 ) ) ;
#1268 = ORIENTED_EDGE ( 'NONE', *, *, #1872, .F. ) ;
#1269 = LINE ( 'NONE', #5767, #1561 ) ;
#1270 = VECTOR ( 'NONE', #890, 1000.000000000000000 ) ;
#1271 = LINE ( 'NONE', #3538, #7254 ) ;
#1272 = ADVANCED_FACE ( 'NONE', ( #7029 ), #146, .F. ) ;
#1273 = CARTESIAN_POINT ( 'NONE',  ( 1.411581201560190495E-15, 4.862606272033091592, -3.745885042887436622 ) ) ;
#1274 = DIRECTION ( 'NONE',  ( -0.000000000000000000, -0.000000000000000000, 1.000000000000000000 ) ) ;
#1275 = ADVANCED_FACE ( 'NONE', ( #4172 ), #5757, .T. ) ;
#1276 = ORIENTED_EDGE ( 'NONE', *, *, #2307, .T. ) ;
#1277 = FACE_OUTER_BOUND ( 'NONE', #3592, .T. ) ;
#1278 = ORIENTED_EDGE ( 'NONE', *, *, #3591, .T. ) ;
#1279 = EDGE_LOOP ( 'NONE', ( #2472, #3546, #4649, #7331 ) ) ;
#1280 = DIRECTION ( 'NONE',  ( 0.000000000000000000, 0.000000000000000000, 1.000000000000000000 ) ) ;
#1281 = CARTESIAN_POINT ( 'NONE',  ( -2.712762565639006418, 3.052587955997511759, -3.430618716626627318 ) ) ;
#1282 = CYLINDRICAL_SURFACE ( 'NONE', #4577, 9.999999999999996447 ) ;
#1283 = DIRECTION ( 'NONE',  ( 0.000000000000000000, 0.000000000000000000, -1.000000000000000000 ) ) ;
#1284 = EDGE_CURVE ( 'NONE', #4530, #1949, #4744, .T. ) ;
#1285 = CARTESIAN_POINT ( 'NONE',  ( 0.000000000000000000, 0.000000000000000000, -140.0000000000000000 ) ) ;
#1286 = EDGE_LOOP ( 'NONE', ( #2523, #5606 ) ) ;
#1287 = ADVANCED_FACE ( 'NONE', ( #6614 ), #7208, .F. ) ;
#1288 = VERTEX_POINT ( 'NONE', #3096 ) ;
#1289 = PRODUCT_DEFINITION_SHAPE ( 'NONE', 'NONE',  #4274 ) ;
#1290 = ITEM_DEFINED_TRANSFORMATION ( 'NONE', 'NONE', #893,  #1963 ) ;
#1291 = DIRECTION ( 'NONE',  ( 0.000000000000000000, -1.000000000000000000, 0.000000000000000000 ) ) ;
#1292 = ORIENTED_EDGE ( 'NONE', *, *, #6513, .T. ) ;
#1293 = EDGE_CURVE ( 'NONE', #3386, #7293, #5516, .T. ) ;
#1294 = CARTESIAN_POINT ( 'NONE',  ( -5.000000000000000888, -8.660254037844389075, 150.0000000000000000 ) ) ;
#1295 = EDGE_LOOP ( 'NONE', ( #2418, #3734, #5993, #5762 ) ) ;
#1296 = EDGE_CURVE ( 'NONE', #5339, #4696, #2111, .T. ) ;
#1297 = FACE_OUTER_BOUND ( 'NONE', #7119, .T. ) ;
#1298 = CARTESIAN_POINT ( 'NONE',  ( 445.0000000000000000, -8.660254037844389075, 140.0000000000000000 ) ) ;
#1299 = DIRECTION ( 'NONE',  ( 0.000000000000000000, 1.000000000000000000, 0.000000000000000000 ) ) ;
#1300 = ORIENTED_EDGE ( 'NONE', *, *, #4328, .F. ) ;
#1301 = DIRECTION ( 'NONE',  ( 1.000000000000000000, 0.000000000000000000, 0.000000000000000000 ) ) ;
#1302 = CARTESIAN_POINT ( 'NONE',  ( -0.1750025118121544265, -4.719839900820635314, -3.469254087858253399 ) ) ;
#1303 = CYLINDRICAL_SURFACE ( 'NONE', #6167, 10.72500000000000142 ) ;
#1304 = VERTEX_POINT ( 'NONE', #3677 ) ;
#1305 = DIRECTION ( 'NONE',  ( -0.000000000000000000, 1.000000000000000000, -0.000000000000000000 ) ) ;
#1306 = EDGE_CURVE ( 'NONE', #5483, #6671, #924, .T. ) ;
#1307 = ORIENTED_EDGE ( 'NONE', *, *, #5165, .T. ) ;
#1308 = VERTEX_POINT ( 'NONE', #5402 ) ;
#1309 = DIRECTION ( 'NONE',  ( 0.000000000000000000, -0.4999999999999993894, 0.8660254037844389297 ) ) ;
#1310 = CARTESIAN_POINT ( 'NONE',  ( -1.390230914382372118, -4.043987460488664532, -3.502507215260523665 ) ) ;
#1311 = CARTESIAN_POINT ( 'NONE',  ( -0.7826237921249277196, 0.000000000000000000, 0.000000000000000000 ) ) ;
#1312 = FACE_OUTER_BOUND ( 'NONE', #6458, .T. ) ;
#1313 = CIRCLE ( 'NONE', #5497, 2.500000000000001332 ) ;
#1314 = DIRECTION ( 'NONE',  ( 0.000000000000000000, -0.000000000000000000, -1.000000000000000000 ) ) ;
#1315 = DIRECTION ( 'NONE',  ( -0.000000000000000000, -0.000000000000000000, 1.000000000000000000 ) ) ;
#1316 = ORIENTED_EDGE ( 'NONE', *, *, #3473, .T. ) ;
#1317 = EDGE_LOOP ( 'NONE', ( #6784, #6485, #783, #2163 ) ) ;
#1318 = EDGE_CURVE ( 'NONE', #2488, #2773, #2508, .T. ) ;
#1319 = CARTESIAN_POINT ( 'NONE',  ( 303.3333333333333144, -20.00000000000000000, 165.1500000000000625 ) ) ;
#1320 = ORIENTED_EDGE ( 'NONE', *, *, #4174, .T. ) ;
#1321 = EDGE_CURVE ( 'NONE', #5898, #3234, #1480, .T. ) ;
#1322 = PRODUCT_DEFINITION_SHAPE ( 'NONE', 'NONE',  #7378 ) ;
#1323 = VECTOR ( 'NONE', #4650, 1000.000000000000000 ) ;
#1324 = CARTESIAN_POINT ( 'NONE',  ( -4.000000000000000000, -0.8382240730041925492, -3.220610619767135141 ) ) ;
#1325 = VERTEX_POINT ( 'NONE', #6660 ) ;
#1326 = ADVANCED_FACE ( 'NONE', ( #2547 ), #1377, .F. ) ;
#1327 = ORIENTED_EDGE ( 'NONE', *, *, #2416, .F. ) ;
#1328 = DIRECTION ( 'NONE',  ( 1.000000000000000000, 0.000000000000000000, 0.000000000000000000 ) ) ;
#1329 = AXIS2_PLACEMENT_3D ( 'NONE', #611, #5171, #52 ) ;
#1330 = CARTESIAN_POINT ( 'NONE',  ( -30.00000000000002842, -20.00000000000000000, 180.0000000000000284 ) ) ;
#1331 = CARTESIAN_POINT ( 'NONE',  ( 386.6666666666666288, -25.00000000000000000, -162.5000000000000853 ) ) ;
#1332 = ORIENTED_EDGE ( 'NONE', *, *, #4834, .F. ) ;
#1333 = AXIS2_PLACEMENT_3D ( 'NONE', #5931, #5284, #1979 ) ;
#1334 = PLANE ( 'NONE',  #607 ) ;
#1335 = B_SPLINE_CURVE_WITH_KNOTS ( 'NONE', 3,
 ( #4464, #3784, #6084, #6684, #3242, #5589, #946, #5429 ),
 .UNSPECIFIED., .F., .F.,
 ( 4, 2, 2, 4 ),
 ( 2.465131517071610173E-07, 0.001183067374689837636, 0.001774477805458902699, 0.002365888236227967761 ),
 .UNSPECIFIED. ) ;
#1336 = ITEM_DEFINED_TRANSFORMATION ( 'NONE', 'NONE', #1601,  #1963 ) ;
#1337 = FACE_OUTER_BOUND ( 'NONE', #3306, .T. ) ;
#1338 = DIRECTION ( 'NONE',  ( 0.000000000000000000, 1.000000000000000000, 0.000000000000000000 ) ) ;
#1339 = DIRECTION ( 'NONE',  ( 1.000000000000000000, 0.000000000000000000, 0.000000000000000000 ) ) ;
#1340 = ORIENTED_EDGE ( 'NONE', *, *, #1164, .T. ) ;
#1341 = LINE ( 'NONE', #3622, #6881 ) ;
#1342 = PRODUCT_DEFINITION_SHAPE ( 'NONE', 'NONE',  #6666 ) ;
#1343 = AXIS2_PLACEMENT_3D ( 'NONE', #3176, #6612, #5478 ) ;
#1344 = VERTEX_POINT ( 'NONE', #5480 ) ;
#1345 = ORIENTED_EDGE ( 'NONE', *, *, #6912, .T. ) ;
#1346 = LINE ( 'NONE', #5282, #4563 ) ;
#1347 = CARTESIAN_POINT ( 'NONE',  ( 219.9999999999999716, -20.00000000000000000, 165.1500000000000625 ) ) ;
#1348 = DIRECTION ( 'NONE',  ( -0.000000000000000000, -0.000000000000000000, -1.000000000000000000 ) ) ;
#1349 = DIRECTION ( 'NONE',  ( 0.000000000000000000, 0.000000000000000000, 1.000000000000000000 ) ) ;
#1350 = VECTOR ( 'NONE', #759, 999.9999999999998863 ) ;
#1351 = AXIS2_PLACEMENT_3D ( 'NONE', #1484, #1562, #1045 ) ;
#1352 = ADVANCED_FACE ( 'NONE', ( #363 ), #4845, .F. ) ;
#1353 = AXIS2_PLACEMENT_3D ( 'NONE', #4354, #3867, #2656 ) ;
#1354 = LINE ( 'NONE', #211, #5662 ) ;
#1355 = CARTESIAN_POINT ( 'NONE',  ( 0.000000000000000000, 1.178949249685213863, -2.042000000000001148 ) ) ;
#1356 = ORIENTED_EDGE ( 'NONE', *, *, #5165, .F. ) ;
#1357 = CIRCLE ( 'NONE', #5191, 2.100000000000000089 ) ;
#1358 = CIRCLE ( 'NONE', #2670, 5.560781378645573980 ) ;
#1359 = AXIS2_PLACEMENT_3D ( 'NONE', #2120, #6070, #1445 ) ;
#1360 = CONTEXT_DEPENDENT_SHAPE_REPRESENTATION ( #294, #3060 ) ;
#1361 = CARTESIAN_POINT ( 'NONE',  ( 164.9999999999999716, -8.660254037844389075, 139.9990000000000236 ) ) ;
#1362 = ORIENTED_EDGE ( 'NONE', *, *, #6828, .F. ) ;
#1363 = VECTOR ( 'NONE', #389, 1000.000000000000000 ) ;
#1364 = EDGE_CURVE ( 'NONE', #2884, #6814, #4018, .T. ) ;
#1365 = FACE_OUTER_BOUND ( 'NONE', #5125, .T. ) ;
#1366 = UNCERTAINTY_MEASURE_WITH_UNIT (LENGTH_MEASURE( 1.000000000000000082E-05 ), #2021, 'distance_accuracy_value', 'NONE');
#1367 = VERTEX_POINT ( 'NONE', #4922 ) ;
#1368 = VECTOR ( 'NONE', #5012, 1000.000000000000000 ) ;
#1369 = ORIENTED_EDGE ( 'NONE', *, *, #2451, .T. ) ;
#1370 = ADVANCED_BREP_SHAPE_REPRESENTATION ( '', ( #794, #1963 ), #5205 ) ;
#1371 = PLANE ( 'NONE',  #5056 ) ;
#1372 = DIRECTION ( 'NONE',  ( 0.000000000000000000, 0.000000000000000000, -1.000000000000000000 ) ) ;
#1373 = EDGE_CURVE ( 'NONE', #7234, #3206, #3142, .T. ) ;
#1374 = ORIENTED_EDGE ( 'NONE', *, *, #5945, .T. ) ;
#1375 = AXIS2_PLACEMENT_3D ( 'NONE', #3460, #1328, #3565 ) ;
#1376 =( NAMED_UNIT ( * ) SI_UNIT ( $, .STERADIAN. ) SOLID_ANGLE_UNIT ( ) );
#1377 = CONICAL_SURFACE ( 'NONE', #3408, 2.059999999999998721, 0.9599310885968738161 ) ;
#1378 = EDGE_LOOP ( 'NONE', ( #1421, #1139, #4693, #6522 ) ) ;
#1379 = FACE_OUTER_BOUND ( 'NONE', #3006, .T. ) ;
#1380 = CARTESIAN_POINT ( 'NONE',  ( 3.436319922986518449, -2.634841920959471562, -3.531542292954761741 ) ) ;
#1381 = DIRECTION ( 'NONE',  ( 0.000000000000000000, 0.000000000000000000, -1.000000000000000000 ) ) ;
#1382 = VERTEX_POINT ( 'NONE', #3213 ) ;
#1383 = CARTESIAN_POINT ( 'NONE',  ( -1.391697335622809950, -4.043246145443391448, -3.503898532754372575 ) ) ;
#1384 = ORIENTED_EDGE ( 'NONE', *, *, #5683, .T. ) ;
#1385 = VECTOR ( 'NONE', #6183, 1000.000000000000000 ) ;
#1386 = PRODUCT_DEFINITION_SHAPE ( 'NONE', 'NONE',  #7390 ) ;
#1387 = ORIENTED_EDGE ( 'NONE', *, *, #4449, .T. ) ;
#1388 =( REPRESENTATION_RELATIONSHIP ('NONE','NONE', #5587, #6025 ) REPRESENTATION_RELATIONSHIP_WITH_TRANSFORMATION ( #121 )SHAPE_REPRESENTATION_RELATIONSHIP( ) );
#1389 = CARTESIAN_POINT ( 'NONE',  ( 2.500000000000000000, 0.000000000000000000, 0.000000000000000000 ) ) ;
#1390 = CARTESIAN_POINT ( 'NONE',  ( 0.1410422978106145031, -4.700232962125109104, -3.687027686973628704 ) ) ;
#1391 = CARTESIAN_POINT ( 'NONE',  ( 275.0000000000000000, -8.660254037844389075, 140.0000000000000000 ) ) ;
#1392 = DIRECTION ( 'NONE',  ( 0.000000000000000000, 1.000000000000000000, -1.224646799147353207E-16 ) ) ;
#1393 = EDGE_CURVE ( 'NONE', #4485, #3484, #3897, .T. ) ;
#1394 = FACE_OUTER_BOUND ( 'NONE', #6543, .T. ) ;
#1395 = CARTESIAN_POINT ( 'NONE',  ( 84.99999999999998579, -8.660254037844389075, 145.0000000000000284 ) ) ;
#1396 = AXIS2_PLACEMENT_3D ( 'NONE', #79, #2338, #4636 ) ;
#1397 = VERTEX_POINT ( 'NONE', #2587 ) ;
#1398 = CONTEXT_DEPENDENT_SHAPE_REPRESENTATION ( #769, #7092 ) ;
#1399 = CARTESIAN_POINT ( 'NONE',  ( -31.74999999999995737, 0.000000000000000000, 0.000000000000000000 ) ) ;
#1400 = EDGE_LOOP ( 'NONE', ( #2, #490, #6515, #775 ) ) ;
#1401 = DIRECTION ( 'NONE',  ( 0.000000000000000000, 0.000000000000000000, -1.000000000000000000 ) ) ;
#1402 = CARTESIAN_POINT ( 'NONE',  ( 0.000000000000000000, -15.00000000000000000, 0.000000000000000000 ) ) ;
#1403 = EDGE_LOOP ( 'NONE', ( #3453, #1257, #1882, #5394 ) ) ;
#1404 = ADVANCED_FACE ( 'NONE', ( #2668, #4206, #6573, #4285, #6502, #1365 ), #3642, .T. ) ;
#1405 = ORIENTED_EDGE ( 'NONE', *, *, #2918, .F. ) ;
#1406 = EDGE_CURVE ( 'NONE', #6247, #5197, #3713, .T. ) ;
#1407 = DIRECTION ( 'NONE',  ( 0.000000000000000000, 0.000000000000000000, 1.000000000000000000 ) ) ;
#1408 = PRODUCT_DEFINITION_SHAPE ( 'NONE', 'NONE',  #7361 ) ;
#1409 = CARTESIAN_POINT ( 'NONE',  ( -4.154094228333736538, -2.398367420967545627, -3.721909803043222276 ) ) ;
#1410 = ADVANCED_FACE ( 'NONE', ( #1005 ), #2214, .T. ) ;
#1411 = VERTEX_POINT ( 'NONE', #882 ) ;
#1412 = DIRECTION ( 'NONE',  ( 0.000000000000000000, -1.287488025362403787E-15, -1.000000000000000000 ) ) ;
#1413 = VERTEX_POINT ( 'NONE', #5442 ) ;
#1414 = EDGE_CURVE ( 'NONE', #7258, #4994, #4883, .T. ) ;
#1415 = DIRECTION ( 'NONE',  ( 0.000000000000000000, 0.000000000000000000, -1.000000000000000000 ) ) ;
#1416 = FACE_OUTER_BOUND ( 'NONE', #251, .T. ) ;
#1417 = FACE_BOUND ( 'NONE', #5353, .T. ) ;
#1418 = DIRECTION ( 'NONE',  ( 6.123233995736766036E-17, -1.000000000000000000, 0.000000000000000000 ) ) ;
#1419 = VERTEX_POINT ( 'NONE', #6696 ) ;
#1420 = DIRECTION ( 'NONE',  ( -1.000000000000000000, 0.000000000000000000, 0.000000000000000000 ) ) ;
#1421 = ORIENTED_EDGE ( 'NONE', *, *, #6, .T. ) ;
#1422 = VERTEX_POINT ( 'NONE', #2114 ) ;
#1423 = EDGE_CURVE ( 'NONE', #3349, #4841, #1557, .T. ) ;
#1424 = FACE_OUTER_BOUND ( 'NONE', #3457, .T. ) ;
#1425 = DIRECTION ( 'NONE',  ( 0.000000000000000000, 1.224646799147351975E-16, 1.000000000000000000 ) ) ;
#1426 = CARTESIAN_POINT ( 'NONE',  ( -4.000000000000000000, -0.3979232138631226823, -3.896351557369779711E-17 ) ) ;
#1427 = DIRECTION ( 'NONE',  ( 0.000000000000000000, 0.000000000000000000, -1.000000000000000000 ) ) ;
#1428 = DIRECTION ( 'NONE',  ( 0.000000000000000000, 0.000000000000000000, 1.000000000000000000 ) ) ;
#1429 = CYLINDRICAL_SURFACE ( 'NONE', #2535, 13.50000000000000355 ) ;
#1430 = APPLICATION_CONTEXT ( 'automotive_design' ) ;
#1431 = ORIENTED_EDGE ( 'NONE', *, *, #6454, .F. ) ;
#1432 = DIRECTION ( 'NONE',  ( -0.000000000000000000, -0.000000000000000000, -1.000000000000000000 ) ) ;
#1433 = LINE ( 'NONE', #6058, #3614 ) ;
#1434 = EDGE_LOOP ( 'NONE', ( #5498, #6028, #3512, #7104 ) ) ;
#1435 = EDGE_CURVE ( 'NONE', #4318, #3965, #2809, .T. ) ;
#1436 =( NAMED_UNIT ( * ) SI_UNIT ( $, .STERADIAN. ) SOLID_ANGLE_UNIT ( ) );
#1437 = VECTOR ( 'NONE', #433, 1000.000000000000000 ) ;
#1438 = DIRECTION ( 'NONE',  ( 0.000000000000000000, 0.000000000000000000, -1.000000000000000000 ) ) ;
#1439 = ORIENTED_EDGE ( 'NONE', *, *, #6730, .T. ) ;
#1440 = DIRECTION ( 'NONE',  ( 1.000000000000000000, 0.000000000000000000, 0.000000000000000000 ) ) ;
#1441 = ORIENTED_EDGE ( 'NONE', *, *, #3560, .T. ) ;
#1442 = PLANE ( 'NONE',  #4244 ) ;
#1443 = VECTOR ( 'NONE', #4126, 1000.000000000000000 ) ;
#1444 = EDGE_CURVE ( 'NONE', #2259, #6037, #1625, .T. ) ;
#1445 = DIRECTION ( 'NONE',  ( 0.000000000000000000, 0.000000000000000000, -1.000000000000000000 ) ) ;
#1446 = EDGE_LOOP ( 'NONE', ( #4100, #4125, #4120, #7273 ) ) ;
#1447 = LINE ( 'NONE', #5489, #857 ) ;
#1448 = CARTESIAN_POINT ( 'NONE',  ( 325.0000000000000000, 8.660254037844390851, 145.0000000000000284 ) ) ;
#1449 = CARTESIAN_POINT ( 'NONE',  ( 219.9999999999999716, -20.00000000000000000, 162.5000000000000853 ) ) ;
#1450 = CARTESIAN_POINT ( 'NONE',  ( 0.000000000000000000, 0.000000000000000000, -123.0000000000000000 ) ) ;
#1451 = ORIENTED_EDGE ( 'NONE', *, *, #5683, .F. ) ;
#1452 = CARTESIAN_POINT ( 'NONE',  ( 0.000000000000000000, 0.000000000000000000, 0.000000000000000000 ) ) ;
#1453 = EDGE_CURVE ( 'NONE', #2910, #7189, #2090, .T. ) ;
#1454 = VECTOR ( 'NONE', #4253, 1000.000000000000000 ) ;
#1455 = EDGE_CURVE ( 'NONE', #598, #3083, #6300, .T. ) ;
#1456 = ORIENTED_EDGE ( 'NONE', *, *, #5758, .T. ) ;
#1457 = ORIENTED_EDGE ( 'NONE', *, *, #5359, .T. ) ;
#1458 = DIRECTION ( 'NONE',  ( -0.000000000000000000, 0.000000000000000000, -1.000000000000000000 ) ) ;
#1459 = CARTESIAN_POINT ( 'NONE',  ( 275.0000000000000000, 8.660254037844390851, 140.0000000000000000 ) ) ;
#1460 = LINE ( 'NONE', #6200, #3483 ) ;
#1461 = CARTESIAN_POINT ( 'NONE',  ( -4.000000000000000888, 1.563622288139195238, -0.2253451193528307472 ) ) ;
#1462 = AXIS2_PLACEMENT_3D ( 'NONE', #2524, #428, #5496 ) ;
#1463 = DIRECTION ( 'NONE',  ( 1.000000000000000000, 0.000000000000000000, 0.000000000000000000 ) ) ;
#1464 = CARTESIAN_POINT ( 'NONE',  ( 0.2500000000000002220, 0.000000000000000000, 0.000000000000000000 ) ) ;
#1465 = DIRECTION ( 'NONE',  ( 0.000000000000000000, 0.000000000000000000, -1.000000000000000000 ) ) ;
#1466 = EDGE_CURVE ( 'NONE', #647, #3098, #2439, .T. ) ;
#1467 = ORIENTED_EDGE ( 'NONE', *, *, #4714, .F. ) ;
#1468 = PRODUCT_DEFINITION_SHAPE ( 'NONE', 'NONE',  #7354 ) ;
#1469 = DIRECTION ( 'NONE',  ( 0.000000000000000000, 0.000000000000000000, 1.000000000000000000 ) ) ;
#1470 = AXIS2_PLACEMENT_3D ( 'NONE', #1940, #5854, #2498 ) ;
#1471 = CARTESIAN_POINT ( 'NONE',  ( -5.000000000000000888, -8.660254037844389075, 150.0000000000000000 ) ) ;
#1472 = AXIS2_PLACEMENT_3D ( 'NONE', #899, #7270, #937 ) ;
#1473 = ORIENTED_EDGE ( 'NONE', *, *, #2995, .F. ) ;
#1474 = DIRECTION ( 'NONE',  ( 0.000000000000000000, 1.000000000000000000, 0.000000000000000000 ) ) ;
#1475 = VECTOR ( 'NONE', #2394, 1000.000000000000000 ) ;
#1476 = PRODUCT_CONTEXT ( 'NONE', #61, 'mechanical' ) ;
#1477 = CARTESIAN_POINT ( 'NONE',  ( -3.974344831685191280E-13, 4.796734841935104576, -3.721909803043223608 ) ) ;
#1478 = AXIS2_PLACEMENT_3D ( 'NONE', #460, #1163, #1054 ) ;
#1479 = DIRECTION ( 'NONE',  ( -0.000000000000000000, -0.000000000000000000, 1.000000000000000000 ) ) ;
#1480 = LINE ( 'NONE', #1954, #5208 ) ;
#1481 = AXIS2_PLACEMENT_3D ( 'NONE', #6686, #1583, #4957 ) ;
#1482 = B_SPLINE_CURVE_WITH_KNOTS ( 'NONE', 3,
 ( #4505, #2730, #4571, #3324 ),
 .UNSPECIFIED., .F., .F.,
 ( 4, 4 ),
 ( 0.000000000000000000, 0.002452478801916361129 ),
 .UNSPECIFIED. ) ;
#1483 = ORIENTED_EDGE ( 'NONE', *, *, #5965, .F. ) ;
#1484 = CARTESIAN_POINT ( 'NONE',  ( 400.0000000000000000, 0.000000000000000000, 0.000000000000000000 ) ) ;
#1485 = ORIENTED_EDGE ( 'NONE', *, *, #3536, .T. ) ;
#1486 = VECTOR ( 'NONE', #2324, 999.9999999999998863 ) ;
#1487 = CARTESIAN_POINT ( 'NONE',  ( 195.0000000000000000, 8.660254037844390851, 139.9990000000000236 ) ) ;
#1488 = CONICAL_SURFACE ( 'NONE', #4955, 4.000000000000000000, 0.8911886515913786111 ) ;
#1489 = PLANE ( 'NONE',  #5904 ) ;
#1490 = AXIS2_PLACEMENT_3D ( 'NONE', #4896, #4987, #2126 ) ;
#1491 = EDGE_LOOP ( 'NONE', ( #1473, #6420, #1799, #636 ) ) ;
#1492 = AXIS2_PLACEMENT_3D ( 'NONE', #4006, #3319, #496 ) ;
#1493 = EDGE_CURVE ( 'NONE', #4461, #4011, #6770, .T. ) ;
#1494 = CARTESIAN_POINT ( 'NONE',  ( 4.000000000000000000, -1.700175430507292473, -3.320327275037661785 ) ) ;
#1495 = PLANE ( 'NONE',  #38 ) ;
#1496 = FACE_OUTER_BOUND ( 'NONE', #5581, .T. ) ;
#1497 = VECTOR ( 'NONE', #2553, 1000.000000000000000 ) ;
#1498 = DIRECTION ( 'NONE',  ( -1.000000000000000000, 0.000000000000000000, 0.000000000000000000 ) ) ;
#1499 = VECTOR ( 'NONE', #3835, 1000.000000000000000 ) ;
#1500 = ORIENTED_EDGE ( 'NONE', *, *, #3316, .T. ) ;
#1501 = FACE_BOUND ( 'NONE', #6434, .T. ) ;
#1502 = VERTEX_POINT ( 'NONE', #2705 ) ;
#1503 = EDGE_CURVE ( 'NONE', #2165, #2018, #5078, .T. ) ;
#1504 = ORIENTED_EDGE ( 'NONE', *, *, #4187, .F. ) ;
#1505 = LINE ( 'NONE', #5966, #133 ) ;
#1506 = AXIS2_PLACEMENT_3D ( 'NONE', #4392, #5658, #5547 ) ;
#1507 = FACE_OUTER_BOUND ( 'NONE', #4241, .T. ) ;
#1508 = CARTESIAN_POINT ( 'NONE',  ( 303.3333333333333144, -20.00000000000000000, -159.8500000000001080 ) ) ;
#1509 = CARTESIAN_POINT ( 'NONE',  ( 0.000000000000000000, 0.000000000000000000, 11.75000000000000000 ) ) ;
#1510 = EDGE_CURVE ( 'NONE', #4492, #3944, #513, .T. ) ;
#1511 = CARTESIAN_POINT ( 'NONE',  ( 2.500000000000000000, 2.357898499370433054, -1.951563910473907981E-15 ) ) ;
#1512 = DIRECTION ( 'NONE',  ( -1.000000000000000000, -0.000000000000000000, -0.000000000000000000 ) ) ;
#1513 = CARTESIAN_POINT ( 'NONE',  ( 386.6666666666666288, -25.00000000000000000, -162.5000000000000853 ) ) ;
#1514 = CIRCLE ( 'NONE', #5449, 10.72500000000000142 ) ;
#1515 = EDGE_LOOP ( 'NONE', ( #2970, #4408 ) ) ;
#1516 = LINE ( 'NONE', #3249, #5156 ) ;
#1517 = DIRECTION ( 'NONE',  ( 0.000000000000000000, 0.000000000000000000, 1.000000000000000000 ) ) ;
#1518 = EDGE_CURVE ( 'NONE', #3217, #1606, #2218, .T. ) ;
#1519 = AXIS2_PLACEMENT_3D ( 'NONE', #3177, #2023, #2070 ) ;
#1520 = APPLICATION_PROTOCOL_DEFINITION ( 'draft international standard', 'automotive_design', 1998, #1430 ) ;
#1521 = CARTESIAN_POINT ( 'NONE',  ( 25.00000000000000000, 2.789133085058098087E-16, -2.055000000000000160 ) ) ;
#1522 = DIRECTION ( 'NONE',  ( -0.000000000000000000, -0.000000000000000000, 1.000000000000000000 ) ) ;
#1523 = VERTEX_POINT ( 'NONE', #6807 ) ;
#1524 = ORIENTED_EDGE ( 'NONE', *, *, #4932, .T. ) ;
#1525 = DIRECTION ( 'NONE',  ( 0.000000000000000000, 0.000000000000000000, 1.000000000000000000 ) ) ;
#1526 = ORIENTED_EDGE ( 'NONE', *, *, #4411, .F. ) ;
#1527 = EDGE_CURVE ( 'NONE', #2818, #1325, #3372, .T. ) ;
#1528 = CARTESIAN_POINT ( 'NONE',  ( 2.499999999999999556, 0.000000000000000000, 3.469446951953614189E-15 ) ) ;
#1529 = CARTESIAN_POINT ( 'NONE',  ( -4.101948962585906244, 2.368261337751074169, -3.681124513963621503 ) ) ;
#1530 = DIRECTION ( 'NONE',  ( -1.000000000000000000, -0.000000000000000000, -0.000000000000000000 ) ) ;
#1531 = ORIENTED_EDGE ( 'NONE', *, *, #3496, .F. ) ;
#1532 = DIRECTION ( 'NONE',  ( 0.000000000000000000, 0.000000000000000000, -1.000000000000000000 ) ) ;
#1533 = ORIENTED_EDGE ( 'NONE', *, *, #2575, .F. ) ;
#1534 = CARTESIAN_POINT ( 'NONE',  ( 195.0000000000000000, -8.660254037844389075, 145.0000000000000284 ) ) ;
#1535 = FACE_BOUND ( 'NONE', #697, .T. ) ;
#1536 = DIRECTION ( 'NONE',  ( 1.000000000000000000, 6.123233995736766036E-17, -6.123233995736764803E-17 ) ) ;
#1537 =( REPRESENTATION_RELATIONSHIP ('NONE','NONE', #5587, #5294 ) REPRESENTATION_RELATIONSHIP_WITH_TRANSFORMATION ( #2732 )SHAPE_REPRESENTATION_RELATIONSHIP( ) );
#1538 = VERTEX_POINT ( 'NONE', #6093 ) ;
#1539 = CARTESIAN_POINT ( 'NONE',  ( -4.211140560182196957, 2.431303136016537803, -3.745885042887433514 ) ) ;
#1540 = ORIENTED_EDGE ( 'NONE', *, *, #235, .F. ) ;
#1541 = ORIENTED_EDGE ( 'NONE', *, *, #6416, .T. ) ;
#1542 = CARTESIAN_POINT ( 'NONE',  ( -5.000000000000000888, -8.660254037844389075, 150.0000000000000000 ) ) ;
#1543 = CARTESIAN_POINT ( 'NONE',  ( 275.0000000000000000, 8.660254037844390851, 139.9990000000000236 ) ) ;
#1544 = ITEM_DEFINED_TRANSFORMATION ( 'NONE', 'NONE', #874,  #1963 ) ;
#1545 = CARTESIAN_POINT ( 'NONE',  ( 1.800000000000002931, 1.653273178848927261E-15, 13.50000000000000178 ) ) ;
#1546 = CARTESIAN_POINT ( 'NONE',  ( 2.000000000000001776, 1.641026710857453312E-15, 13.29999999999999893 ) ) ;
#1547 = CARTESIAN_POINT ( 'NONE',  ( 0.000000000000000000, 0.000000000000000000, 121.0000000000000000 ) ) ;
#1548 = CARTESIAN_POINT ( 'NONE',  ( 0.000000000000000000, 0.000000000000000000, -150.0000000000000000 ) ) ;
#1549 = ADVANCED_FACE ( 'NONE', ( #1038, #3828 ), #6127, .T. ) ;
#1550 = VERTEX_POINT ( 'NONE', #3299 ) ;
#1551 = CARTESIAN_POINT ( 'NONE',  ( 0.000000000000000000, 0.000000000000000000, 125.0000000000000000 ) ) ;
#1552 = DIRECTION ( 'NONE',  ( -0.000000000000000000, 1.000000000000000000, -0.000000000000000000 ) ) ;
#1553 = DIRECTION ( 'NONE',  ( 0.000000000000000000, -1.000000000000000000, 0.000000000000000000 ) ) ;
#1554 = CARTESIAN_POINT ( 'NONE',  ( 4.999999999999999112, 8.660254037844390851, 140.0000000000000000 ) ) ;
#1555 =( LENGTH_UNIT ( ) NAMED_UNIT ( * ) SI_UNIT ( .MILLI., .METRE. ) );
#1556 = DIRECTION ( 'NONE',  ( 0.000000000000000000, 0.000000000000000000, 1.000000000000000000 ) ) ;
#1557 = LINE ( 'NONE', #4406, #1499 ) ;
#1558 = ADVANCED_FACE ( 'NONE', ( #289 ), #3929, .F. ) ;
#1559 = EDGE_LOOP ( 'NONE', ( #4249, #164, #4770 ) ) ;
#1560 = ORIENTED_EDGE ( 'NONE', *, *, #1073, .F. ) ;
#1561 = VECTOR ( 'NONE', #7037, 1000.000000000000000 ) ;
#1562 = DIRECTION ( 'NONE',  ( 0.000000000000000000, 0.000000000000000000, 1.000000000000000000 ) ) ;
#1563 = VERTEX_POINT ( 'NONE', #1628 ) ;
#1564 = DIRECTION ( 'NONE',  ( 0.000000000000000000, -1.000000000000000000, 0.000000000000000000 ) ) ;
#1565 = CARTESIAN_POINT ( 'NONE',  ( -4.024497503033519941, 2.323544716729375459, -3.572167766733379768 ) ) ;
#1566 = CARTESIAN_POINT ( 'NONE',  ( 2.500000000000000000, 1.768423874527824902, 1.020999999999999019 ) ) ;
#1567 = EDGE_CURVE ( 'NONE', #7307, #4268, #398, .T. ) ;
#1568 = EDGE_LOOP ( 'NONE', ( #3636, #7115, #3421, #1201 ) ) ;
#1569 = AXIS2_PLACEMENT_3D ( 'NONE', #7251, #7325, #5370 ) ;
#1570 = PLANE ( 'NONE',  #537 ) ;
#1571 = EDGE_CURVE ( 'NONE', #3704, #2028, #6180, .T. ) ;
#1572 = DIRECTION ( 'NONE',  ( -0.000000000000000000, 1.000000000000000000, -0.000000000000000000 ) ) ;
#1573 = DIRECTION ( 'NONE',  ( 1.000000000000000000, 0.000000000000000000, 0.000000000000000000 ) ) ;
#1574 = DIRECTION ( 'NONE',  ( 1.000000000000000000, 6.123233995736766036E-17, -6.123233995736764803E-17 ) ) ;
#1575 = EDGE_LOOP ( 'NONE', ( #2528, #2343, #3084, #1186, #7271, #6192, #1345 ) ) ;
#1576 = CARTESIAN_POINT ( 'NONE',  ( 0.000000000000000000, 0.000000000000000000, 0.000000000000000000 ) ) ;
#1577 = ORIENTED_EDGE ( 'NONE', *, *, #3686, .T. ) ;
#1578 = ORIENTED_EDGE ( 'NONE', *, *, #3283, .T. ) ;
#1579 = DIRECTION ( 'NONE',  ( 0.000000000000000000, 0.000000000000000000, 1.000000000000000000 ) ) ;
#1580 = CARTESIAN_POINT ( 'NONE',  ( 3.453038570460273071, 2.625189405340834448, -3.535263753543585352 ) ) ;
#1581 = CARTESIAN_POINT ( 'NONE',  ( 2.500000000000000000, -1.178949249685213863, 2.042000000000002924 ) ) ;
#1582 = LINE ( 'NONE', #4953, #5915 ) ;
#1583 = DIRECTION ( 'NONE',  ( -0.000000000000000000, 1.000000000000000000, -0.000000000000000000 ) ) ;
#1584 = UNCERTAINTY_MEASURE_WITH_UNIT (LENGTH_MEASURE( 1.000000000000000082E-05 ), #6374, 'distance_accuracy_value', 'NONE');
#1585 = DIRECTION ( 'NONE',  ( -0.000000000000000000, -1.000000000000000000, -0.000000000000000000 ) ) ;
#1586 = ORIENTED_EDGE ( 'NONE', *, *, #7280, .F. ) ;
#1587 = VECTOR ( 'NONE', #3164, 1000.000000000000000 ) ;
#1588 = LINE ( 'NONE', #6605, #5266 ) ;
#1589 = CARTESIAN_POINT ( 'NONE',  ( 303.3333333333333144, -15.00000000000000000, 162.5000000000000853 ) ) ;
#1590 = EDGE_CURVE ( 'NONE', #6398, #1084, #1036, .T. ) ;
#1591 = CARTESIAN_POINT ( 'NONE',  ( 0.000000000000000000, 0.000000000000000000, -4.974599999999998801 ) ) ;
#1592 = DIRECTION ( 'NONE',  ( 0.000000000000000000, 0.000000000000000000, -1.000000000000000000 ) ) ;
#1593 = DIRECTION ( 'NONE',  ( -0.000000000000000000, -0.000000000000000000, 1.000000000000000000 ) ) ;
#1594 = ORIENTED_EDGE ( 'NONE', *, *, #4111, .T. ) ;
#1595 = CIRCLE ( 'NONE', #4586, 0.2000000000000022593 ) ;
#1596 = VERTEX_POINT ( 'NONE', #2740 ) ;
#1597 = DIRECTION ( 'NONE',  ( 6.123233995736766036E-17, -1.000000000000000000, 0.000000000000000000 ) ) ;
#1598 = VERTEX_POINT ( 'NONE', #2108 ) ;
#1599 = CARTESIAN_POINT ( 'NONE',  ( -30.00000000000002842, -25.00000000000000000, -200.0000000000000000 ) ) ;
#1600 = ADVANCED_FACE ( 'NONE', ( #5040 ), #5631, .F. ) ;
#1601 = AXIS2_PLACEMENT_3D ( 'NONE', #3180, #5482, #3715 ) ;
#1602 = B_SPLINE_CURVE_WITH_KNOTS ( 'NONE', 3,
 ( #5624, #1725, #4016, #6228, #6340 ),
 .UNSPECIFIED., .F., .F.,
 ( 4, 1, 4 ),
 ( 0.000000000000000000, 0.002309401076758505356, 0.004618802153517010713 ),
 .UNSPECIFIED. ) ;
#1603 = AXIS2_PLACEMENT_3D ( 'NONE', #2576, #2138, #7243 ) ;
#1604 = CARTESIAN_POINT ( 'NONE',  ( 435.0000000000000568, 8.660254037844390851, 139.9990000000000236 ) ) ;
#1605 = CARTESIAN_POINT ( 'NONE',  ( 53.33333333333330017, -20.00000000000000000, 162.5000000000000853 ) ) ;
#1606 = VERTEX_POINT ( 'NONE', #5560 ) ;
#1607 = AXIS2_PLACEMENT_3D ( 'NONE', #5888, #4687, #5358 ) ;
#1608 = DIRECTION ( 'NONE',  ( -1.000000000000000000, -0.000000000000000000, -0.000000000000000000 ) ) ;
#1609 = FACE_OUTER_BOUND ( 'NONE', #2982, .T. ) ;
#1610 = ADVANCED_FACE ( 'NONE', ( #7323 ), #998, .F. ) ;
#1611 = DIRECTION ( 'NONE',  ( 1.000000000000000000, 0.000000000000000000, 0.000000000000000000 ) ) ;
#1612 = VERTEX_POINT ( 'NONE', #6278 ) ;
#1613 = EDGE_CURVE ( 'NONE', #1502, #2383, #6056, .T. ) ;
#1614 = ORIENTED_EDGE ( 'NONE', *, *, #2679, .F. ) ;
#1615 = ORIENTED_EDGE ( 'NONE', *, *, #5724, .T. ) ;
#1616 = CARTESIAN_POINT ( 'NONE',  ( 53.33333333333330017, -20.00000000000000000, 159.8500000000001080 ) ) ;
#1617 = PLANE ( 'NONE',  #321 ) ;
#1618 = VECTOR ( 'NONE', #2592, 1000.000000000000000 ) ;
#1619 = LINE ( 'NONE', #645, #4087 ) ;
#1620 = DIRECTION ( 'NONE',  ( 0.000000000000000000, -1.224646799147353454E-16, 1.000000000000000000 ) ) ;
#1621 = CARTESIAN_POINT ( 'NONE',  ( -20.63749999999999574, 0.000000000000000000, -12.44999999999999929 ) ) ;
#1622 = DIRECTION ( 'NONE',  ( 1.000000000000000000, 0.000000000000000000, 0.000000000000000000 ) ) ;
#1623 = VECTOR ( 'NONE', #2260, 1000.000000000000000 ) ;
#1624 = ORIENTED_EDGE ( 'NONE', *, *, #337, .T. ) ;
#1625 = CIRCLE ( 'NONE', #5693, 2.649999999999985700 ) ;
#1626 = ADVANCED_FACE ( 'NONE', ( #5179 ), #618, .F. ) ;
#1627 = DIRECTION ( 'NONE',  ( -0.000000000000000000, 1.000000000000000000, 0.000000000000000000 ) ) ;
#1628 = CARTESIAN_POINT ( 'NONE',  ( 1.799999999999996048, 1.236893267138826416E-15, 9.999999999999994671 ) ) ;
#1629 = DIRECTION ( 'NONE',  ( -0.000000000000000000, 0.000000000000000000, 1.000000000000000000 ) ) ;
#1630 = CARTESIAN_POINT ( 'NONE',  ( 4.999999999999999112, 8.660254037844390851, 145.0000000000000284 ) ) ;
#1631 = AXIS2_PLACEMENT_3D ( 'NONE', #5110, #4074, #120 ) ;
#1632 = FACE_OUTER_BOUND ( 'NONE', #1559, .T. ) ;
#1633 = ORIENTED_EDGE ( 'NONE', *, *, #7098, .F. ) ;
#1634 = ORIENTED_EDGE ( 'NONE', *, *, #6220, .T. ) ;
#1636 = AXIS2_PLACEMENT_3D ( 'NONE', #6819, #1158, #7338 ) ;
#1635 = DIRECTION ( 'NONE',  ( 0.000000000000000000, 0.000000000000000000, 1.000000000000000000 ) ) ;
#1637 = ORIENTED_EDGE ( 'NONE', *, *, #7141, .T. ) ;
#1638 =( REPRESENTATION_RELATIONSHIP ('NONE','NONE', #5587, #5023 ) REPRESENTATION_RELATIONSHIP_WITH_TRANSFORMATION ( #5895 )SHAPE_REPRESENTATION_RELATIONSHIP( ) );
#1639 = DIRECTION ( 'NONE',  ( 0.000000000000000000, -0.000000000000000000, -1.000000000000000000 ) ) ;
#1640 = CARTESIAN_POINT ( 'NONE',  ( 2.500000000000000444, 0.000000000000000000, -25.03750572909317285 ) ) ;
#1641 = EDGE_CURVE ( 'NONE', #6814, #630, #6528, .T. ) ;
#1642 = ORIENTED_EDGE ( 'NONE', *, *, #5048, .F. ) ;
#1643 = CIRCLE ( 'NONE', #2578, 2.649999999999985700 ) ;
#1644 = DIRECTION ( 'NONE',  ( 0.000000000000000000, 0.000000000000000000, 1.000000000000000000 ) ) ;
#1645 = FACE_OUTER_BOUND ( 'NONE', #6486, .T. ) ;
#1646 = CARTESIAN_POINT ( 'NONE',  ( 84.99999999999998579, 8.660254037844390851, 139.9990000000000236 ) ) ;
#1647 = CARTESIAN_POINT ( 'NONE',  ( 53.33333333333330017, -30.00000000000000355, -162.5000000000000853 ) ) ;
#1648 = ORIENTED_EDGE ( 'NONE', *, *, #3152, .T. ) ;
#1649 = DIRECTION ( 'NONE',  ( -0.000000000000000000, -0.000000000000000000, 1.000000000000000000 ) ) ;
#1650 = EDGE_CURVE ( 'NONE', #1304, #6651, #5323, .T. ) ;
#1651 = ORIENTED_EDGE ( 'NONE', *, *, #5306, .F. ) ;
#1652 = VERTEX_POINT ( 'NONE', #6346 ) ;
#1653 = EDGE_CURVE ( 'NONE', #977, #2773, #5851, .T. ) ;
#1654 = DIRECTION ( 'NONE',  ( -0.000000000000000000, 0.000000000000000000, 1.000000000000000000 ) ) ;
#1655 = CARTESIAN_POINT ( 'NONE',  ( 53.33333333333330017, -14.99999999999999822, 162.5000000000000853 ) ) ;
#1656 = CONTEXT_DEPENDENT_SHAPE_REPRESENTATION ( #5985, #3803 ) ;
#1657 = DIRECTION ( 'NONE',  ( 0.000000000000000000, -1.000000000000000000, 0.000000000000000000 ) ) ;
#1658 = CARTESIAN_POINT ( 'NONE',  ( 365.0000000000000000, 8.660254037844390851, 145.0000000000000284 ) ) ;
#1659 = ORIENTED_EDGE ( 'NONE', *, *, #727, .T. ) ;
#1660 = CARTESIAN_POINT ( 'NONE',  ( -1.999999999999998224, 0.000000000000000000, 0.000000000000000000 ) ) ;
#1661 = EDGE_CURVE ( 'NONE', #7340, #1770, #6652, .T. ) ;
#1662 = EDGE_LOOP ( 'NONE', ( #6100, #5267, #1842, #3450 ) ) ;
#1663 = CARTESIAN_POINT ( 'NONE',  ( 53.33333333333330017, -20.00000000000000000, 162.5000000000000853 ) ) ;
#1664 = DIRECTION ( 'NONE',  ( 0.000000000000000000, 0.000000000000000000, 1.000000000000000000 ) ) ;
#1665 = DIRECTION ( 'NONE',  ( -0.5000000000000051070, 1.060575238724903217E-16, -0.8660254037844355990 ) ) ;
#1666 = FACE_BOUND ( 'NONE', #4720, .T. ) ;
#1667 = PRODUCT_DEFINITION ( 'UNKNOWN', '', #5185, #989 ) ;
#1668 = ORIENTED_EDGE ( 'NONE', *, *, #778, .T. ) ;
#1669 = EDGE_LOOP ( 'NONE', ( #4546, #3216, #1776, #6910 ) ) ;
#1670 = ORIENTED_EDGE ( 'NONE', *, *, #575, .T. ) ;
#1671 = CARTESIAN_POINT ( 'NONE',  ( -1.800000000000001155, 0.000000000000000000, 0.000000000000000000 ) ) ;
#1672 = CARTESIAN_POINT ( 'NONE',  ( 1.747541505913279281, -3.837784562140273081, -3.503702292528912299 ) ) ;
#1673 = AXIS2_PLACEMENT_3D ( 'NONE', #4611, #1579, #681 ) ;
#1674 = ORIENTED_EDGE ( 'NONE', *, *, #5009, .T. ) ;
#1675 = DIRECTION ( 'NONE',  ( 1.000000000000000000, 0.000000000000000000, 0.000000000000000000 ) ) ;
#1676 = DIRECTION ( 'NONE',  ( 0.000000000000000000, -1.000000000000000000, 0.000000000000000000 ) ) ;
#1677 = ADVANCED_FACE ( 'NONE', ( #2284 ), #4685, .T. ) ;
#1678 = CYLINDRICAL_SURFACE ( 'NONE', #3640, 12.77499999999999858 ) ;
#1679 = VECTOR ( 'NONE', #4012, 1000.000000000000000 ) ;
#1680 = CARTESIAN_POINT ( 'NONE',  ( 40.00000000000000000, 0.000000000000000000, 123.0000000000000000 ) ) ;
#1681 = EDGE_LOOP ( 'NONE', ( #3263, #1966, #884, #6972 ) ) ;
#1682 = DIRECTION ( 'NONE',  ( 1.000000000000000000, 0.000000000000000000, 0.000000000000000000 ) ) ;
#1683 = VECTOR ( 'NONE', #2914, 1000.000000000000000 ) ;
#1684 = CIRCLE ( 'NONE', #5868, 2.649999999999985700 ) ;
#1685 = ORIENTED_EDGE ( 'NONE', *, *, #5635, .F. ) ;
#1686 = DIRECTION ( 'NONE',  ( -1.000000000000000000, 0.000000000000000000, -0.000000000000000000 ) ) ;
#1687 = LINE ( 'NONE', #6264, #5936 ) ;
#1688 = CARTESIAN_POINT ( 'NONE',  ( 2.500000000000000000, 1.178949249685218525, 2.041999999999999371 ) ) ;
#1689 = CARTESIAN_POINT ( 'NONE',  ( -20.63749999999999929, 0.000000000000000000, -9.999999999999996447 ) ) ;
#1690 = EDGE_CURVE ( 'NONE', #2383, #1502, #2328, .T. ) ;
#1691 = ORIENTED_EDGE ( 'NONE', *, *, #6926, .T. ) ;
#1692 = DIRECTION ( 'NONE',  ( 1.000000000000000000, 0.000000000000000000, 0.000000000000000000 ) ) ;
#1693 = EDGE_CURVE ( 'NONE', #2821, #2892, #6895, .T. ) ;
#1694 = EDGE_LOOP ( 'NONE', ( #2131, #741, #3922, #2257 ) ) ;
#1695 = DIRECTION ( 'NONE',  ( -0.000000000000000000, 1.000000000000000000, -0.000000000000000000 ) ) ;
#1696 = DIRECTION ( 'NONE',  ( -0.8191520442889902442, 0.000000000000000000, -0.5735764363510482688 ) ) ;
#1697 = CARTESIAN_POINT ( 'NONE',  ( 219.9999999999999716, -20.00000000000000000, -162.5000000000000853 ) ) ;
#1698 = CARTESIAN_POINT ( 'NONE',  ( 53.33333333333330017, -20.00000000000000000, 165.1500000000000625 ) ) ;
#1699 = ADVANCED_FACE ( 'NONE', ( #5779 ), #4127, .T. ) ;
#1700 = B_SPLINE_CURVE_WITH_KNOTS ( 'NONE', 3,
 ( #4240, #4281, #5938, #3063, #6571, #4202, #766, #5331 ),
 .UNSPECIFIED., .F., .F.,
 ( 4, 2, 2, 4 ),
 ( 7.780516681398759253E-20, 0.002450665683189819696, 0.003675998524784729327, 0.004901331366379639391 ),
 .UNSPECIFIED. ) ;
#1701 =( NAMED_UNIT ( * ) PLANE_ANGLE_UNIT ( ) SI_UNIT ( $, .RADIAN. ) );
#1702 = ORIENTED_EDGE ( 'NONE', *, *, #6260, .T. ) ;
#1703 = DIRECTION ( 'NONE',  ( -1.000000000000000000, 0.000000000000000000, 0.000000000000000000 ) ) ;
#1704 = ORIENTED_EDGE ( 'NONE', *, *, #4846, .T. ) ;
#1705 = FACE_OUTER_BOUND ( 'NONE', #3662, .T. ) ;
#1706 = VECTOR ( 'NONE', #7328, 1000.000000000000000 ) ;
#1707 = CARTESIAN_POINT ( 'NONE',  ( -1.799999999999996048, 0.000000000000000000, -9.999999999999998224 ) ) ;
#1708 =( BOUNDED_SURFACE ( )  B_SPLINE_SURFACE ( 3, 2, ( 
 ( #5988, #6032, #375 ),
 ( #1494, #4936, #7073 ),
 ( #339, #1967, #6073 ),
 ( #848, #2638, #3106 ),
 ( #7224, #1921, #4220 ),
 ( #5649, #4004, #2235 ) ),
 .UNSPECIFIED., .F., .F., .T. ) 
 B_SPLINE_SURFACE_WITH_KNOTS ( ( 4, 2, 4 ),
 ( 3, 3 ),
 ( 0.02027065861071770947, 0.02273072267836921331, 0.02519078674602071716 ),
 ( 0.000000000000000000, 1.000000000000000000 ),
 .UNSPECIFIED. ) 
 GEOMETRIC_REPRESENTATION_ITEM ( )  RATIONAL_B_SPLINE_SURFACE ( (
 ( 1.000000000000000000, 0.8047781708337304885, 1.000000000000000000),
 ( 1.000000000000000000, 0.8123765190705307671, 1.000000000000000000),
 ( 1.000000000000000000, 0.8190656277163975707, 1.000000000000000000),
 ( 1.000000000000000000, 0.8192366903512159348, 1.000000000000000000),
 ( 1.000000000000000000, 0.8126138454302893610, 1.000000000000000000),
 ( 1.000000000000000000, 0.8047712246031417660, 1.000000000000000000) ) ) 
 REPRESENTATION_ITEM ( '' )  SURFACE ( )  );
#1709 = ORIENTED_EDGE ( 'NONE', *, *, #1466, .T. ) ;
#1710 = EDGE_CURVE ( 'NONE', #3158, #6404, #5216, .T. ) ;
#1711 = DIRECTION ( 'NONE',  ( 0.000000000000000000, 1.000000000000000000, 0.000000000000000000 ) ) ;
#1712 = AXIS2_PLACEMENT_3D ( 'NONE', #2713, #6617, #4974 ) ;
#1713 = LINE ( 'NONE', #5614, #551 ) ;
#1714 = CIRCLE ( 'NONE', #3743, 2.649999999999985700 ) ;
#1715 = CIRCLE ( 'NONE', #437, 1.050000000000000488 ) ;
#1716 = CLOSED_SHELL ( 'NONE', ( #378, #6599, #1410, #865, #6050, #2554, #4984, #5391, #6299, #6148, #5424, #3936, #602, #6504, #3955, #3007, #4029, #3482, #2873, #132, #2862, #187, #6918, #5243, #567, #2597, #5636, #4148 ) ) ;
#1717 = DIRECTION ( 'NONE',  ( 0.000000000000000000, 0.000000000000000000, 1.000000000000000000 ) ) ;
#1718 = ORIENTED_EDGE ( 'NONE', *, *, #4396, .T. ) ;
#1719 = CARTESIAN_POINT ( 'NONE',  ( -5.000000000000000888, -8.660254037844389075, 150.0000000000000000 ) ) ;
#1720 =( REPRESENTATION_RELATIONSHIP ('NONE','NONE', #5587, #951 ) REPRESENTATION_RELATIONSHIP_WITH_TRANSFORMATION ( #4573 )SHAPE_REPRESENTATION_RELATIONSHIP( ) );
#1721 = AXIS2_PLACEMENT_3D ( 'NONE', #6193, #7200, #2056 ) ;
#1722 = ORIENTED_EDGE ( 'NONE', *, *, #2701, .T. ) ;
#1723 = CARTESIAN_POINT ( 'NONE',  ( 10.00000000000000000, 1.224646799147353256E-15, 140.0000000000000000 ) ) ;
#1724 = CARTESIAN_POINT ( 'NONE',  ( 136.6666666666666288, -14.99999999999999822, 159.8500000000001080 ) ) ;
#1725 = CARTESIAN_POINT ( 'NONE',  ( 3.333333333333332593, 2.694301256218250007, -3.300726591567078483 ) ) ;
#1726 = DIRECTION ( 'NONE',  ( -0.000000000000000000, 1.000000000000000000, 1.224646799147353207E-16 ) ) ;
#1727 = VECTOR ( 'NONE', #5465, 1000.000000000000000 ) ;
#1728 = VERTEX_POINT ( 'NONE', #4651 ) ;
#1729 = DIRECTION ( 'NONE',  ( 0.000000000000000000, 1.000000000000000000, 0.000000000000000000 ) ) ;
#1730 = EDGE_CURVE ( 'NONE', #5656, #6176, #4084, .T. ) ;
#1731 = VERTEX_POINT ( 'NONE', #1459 ) ;
#1732 = CIRCLE ( 'NONE', #3884, 13.50000000000000000 ) ;
#1733 = ADVANCED_FACE ( 'NONE', ( #1935 ), #3086, .F. ) ;
#1734 = AXIS2_PLACEMENT_3D ( 'NONE', #528, #1256, #731 ) ;
#1735 = DIRECTION ( 'NONE',  ( 0.000000000000000000, 0.000000000000000000, 1.000000000000000000 ) ) ;
#1736 = CARTESIAN_POINT ( 'NONE',  ( -0.5276280594146446346, 4.314175951381965746, -3.320322319201721495 ) ) ;
#1737 = DIRECTION ( 'NONE',  ( -0.000000000000000000, 1.000000000000000000, -0.000000000000000000 ) ) ;
#1738 = CARTESIAN_POINT ( 'NONE',  ( 1.999999999999994893, 0.000000000000000000, 0.000000000000000000 ) ) ;
#1739 = AXIS2_PLACEMENT_3D ( 'NONE', #3605, #4103, #5761 ) ;
#1740 = CARTESIAN_POINT ( 'NONE',  ( -30.00000000000002842, -25.00000000000000000, -200.0000000000000000 ) ) ;
#1741 = AXIS2_PLACEMENT_3D ( 'NONE', #5744, #3477, #6877 ) ;
#1742 = ORIENTED_EDGE ( 'NONE', *, *, #2024, .T. ) ;
#1743 = ADVANCED_FACE ( 'NONE', ( #4907 ), #907, .T. ) ;
#1744 = PRODUCT_CONTEXT ( 'NONE', #1430, 'mechanical' ) ;
#1745 = ORIENTED_EDGE ( 'NONE', *, *, #3426, .T. ) ;
#1746 = VECTOR ( 'NONE', #2696, 1000.000000000000000 ) ;
#1747 =( NAMED_UNIT ( * ) SI_UNIT ( $, .STERADIAN. ) SOLID_ANGLE_UNIT ( ) );
#1748 = DIRECTION ( 'NONE',  ( 0.000000000000000000, 0.000000000000000000, 1.000000000000000000 ) ) ;
#1749 = CONICAL_SURFACE ( 'NONE', #87, 5.560781378645573980, 1.221730476396046816 ) ;
#1750 = ORIENTED_EDGE ( 'NONE', *, *, #3332, .F. ) ;
#1751 = ADVANCED_FACE ( 'NONE', ( #2609 ), #4497, .F. ) ;
#1752 = DIRECTION ( 'NONE',  ( 1.000000000000000000, 0.000000000000000000, 0.000000000000000000 ) ) ;
#1753 = CARTESIAN_POINT ( 'NONE',  ( 0.000000000000000000, 0.000000000000000000, -4.000000000000000000 ) ) ;
#1754 = ORIENTED_EDGE ( 'NONE', *, *, #3222, .F. ) ;
#1755 = LINE ( 'NONE', #6793, #3009 ) ;
#1756 = ORIENTED_EDGE ( 'NONE', *, *, #4834, .T. ) ;
#1757 = PLANE ( 'NONE',  #880 ) ;
#1758 = DIRECTION ( 'NONE',  ( -1.000000000000000000, 0.000000000000000000, -0.000000000000000000 ) ) ;
#1759 = DIRECTION ( 'NONE',  ( 1.000000000000000000, 0.000000000000000000, 0.000000000000000000 ) ) ;
#1760 = PLANE ( 'NONE',  #4967 ) ;
#1761 = ORIENTED_EDGE ( 'NONE', *, *, #6890, .T. ) ;
#1762 = FACE_OUTER_BOUND ( 'NONE', #2193, .T. ) ;
#1763 = EDGE_LOOP ( 'NONE', ( #5244, #4423 ) ) ;
#1764 = DIRECTION ( 'NONE',  ( 0.000000000000000000, 0.000000000000000000, 1.000000000000000000 ) ) ;
#1765 = DIRECTION ( 'NONE',  ( 1.000000000000000000, 0.000000000000000000, 0.000000000000000000 ) ) ;
#1766 = CYLINDRICAL_SURFACE ( 'NONE', #5756, 2.649999999999985700 ) ;
#1767 = CARTESIAN_POINT ( 'NONE',  ( 136.6666666666666288, -20.00000000000000000, 165.1500000000000625 ) ) ;
#1768 = EDGE_CURVE ( 'NONE', #7293, #1308, #315, .T. ) ;
#1769 =( REPRESENTATION_RELATIONSHIP ('NONE','NONE', #5587, #5023 ) REPRESENTATION_RELATIONSHIP_WITH_TRANSFORMATION ( #2867 )SHAPE_REPRESENTATION_RELATIONSHIP( ) );
#1770 = VERTEX_POINT ( 'NONE', #6564 ) ;
#1771 = APPLICATION_PROTOCOL_DEFINITION ( 'draft international standard', 'automotive_design', 1998, #6186 ) ;
#1772 = VERTEX_POINT ( 'NONE', #6001 ) ;
#1773 =( NAMED_UNIT ( * ) SI_UNIT ( $, .STERADIAN. ) SOLID_ANGLE_UNIT ( ) );
#1774 = EDGE_CURVE ( 'NONE', #5766, #380, #5098, .T. ) ;
#1775 = FACE_OUTER_BOUND ( 'NONE', #519, .T. ) ;
#1776 = ORIENTED_EDGE ( 'NONE', *, *, #4734, .F. ) ;
#1777 = FILL_AREA_STYLE ('',( #6925 ) ) ;
#1778 = CARTESIAN_POINT ( 'NONE',  ( 45.00000000000000000, -8.660254037844389075, 139.9990000000000236 ) ) ;
#1779 = ADVANCED_FACE ( 'NONE', ( #3014 ), #3738, .F. ) ;
#1780 = VERTEX_POINT ( 'NONE', #4271 ) ;
#1781 = FILL_AREA_STYLE ('',( #4639 ) ) ;
#1782 = VERTEX_POINT ( 'NONE', #239 ) ;
#1783 = EDGE_CURVE ( 'NONE', #2951, #7258, #5967, .T. ) ;
#1784 = VERTEX_POINT ( 'NONE', #1347 ) ;
#1785 = DIRECTION ( 'NONE',  ( 0.000000000000000000, -1.000000000000000000, 0.000000000000000000 ) ) ;
#1786 = DIRECTION ( 'NONE',  ( -0.000000000000000000, 0.000000000000000000, 1.000000000000000000 ) ) ;
#1787 = CARTESIAN_POINT ( 'NONE',  ( -5.000000000000000888, -8.660254037844389075, 140.0000000000000000 ) ) ;
#1788 = CARTESIAN_POINT ( 'NONE',  ( -20.63749999999999929, 0.000000000000000000, 0.000000000000000000 ) ) ;
#1789 = ORIENTED_EDGE ( 'NONE', *, *, #67, .T. ) ;
#1790 = CARTESIAN_POINT ( 'NONE',  ( 0.000000000000000000, 0.000000000000000000, 0.000000000000000000 ) ) ;
#1791 = ORIENTED_EDGE ( 'NONE', *, *, #5133, .T. ) ;
#1792 = LINE ( 'NONE', #3547, #1443 ) ;
#1793 = DIRECTION ( 'NONE',  ( 0.000000000000000000, -0.000000000000000000, -1.000000000000000000 ) ) ;
#1794 = DIRECTION ( 'NONE',  ( -0.000000000000000000, 1.000000000000000000, -0.000000000000000000 ) ) ;
#1795 = CARTESIAN_POINT ( 'NONE',  ( -1.655952806101422814, 3.662737355149034979, -7.623296525288699970E-18 ) ) ;
#1796 = VECTOR ( 'NONE', #7286, 1000.000000000000000 ) ;
#1797 = LINE ( 'NONE', #5891, #1350 ) ;
#1798 = ORIENTED_EDGE ( 'NONE', *, *, #2307, .F. ) ;
#1799 = ORIENTED_EDGE ( 'NONE', *, *, #593, .F. ) ;
#1800 = EDGE_CURVE ( 'NONE', #6816, #271, #7127, .T. ) ;
#1801 = CONTEXT_DEPENDENT_SHAPE_REPRESENTATION ( #631, #6021 ) ;
#1802 = PLANE ( 'NONE',  #4219 ) ;
#1803 = ORIENTED_EDGE ( 'NONE', *, *, #462, .T. ) ;
#1804 = AXIS2_PLACEMENT_3D ( 'NONE', #821, #6480, #1887 ) ;
#1805 = CARTESIAN_POINT ( 'NONE',  ( -4.000000000000000000, 0.8730739991738342143, -3.223134629628428893 ) ) ;
#1806 = AXIS2_PLACEMENT_3D ( 'NONE', #3314, #5613, #7267 ) ;
#1807 = EDGE_LOOP ( 'NONE', ( #1198, #3974, #6007, #523 ) ) ;
#1808 = EDGE_CURVE ( 'NONE', #2174, #3114, #1962, .T. ) ;
#1809 = PRODUCT_DEFINITION_SHAPE ( 'NONE', 'NONE',  #7362 ) ;
#1810 = CARTESIAN_POINT ( 'NONE',  ( 3.678949249685231848, 0.000000000000000000, 0.000000000000000000 ) ) ;
#1811 = VECTOR ( 'NONE', #1305, 1000.000000000000000 ) ;
#1812 = CARTESIAN_POINT ( 'NONE',  ( 155.0000000000000000, -8.660254037844389075, 145.0000000000000284 ) ) ;
#1813 = CARTESIAN_POINT ( 'NONE',  ( -1.800000000000002931, 0.000000000000000000, 0.000000000000000000 ) ) ;
#1814 = ORIENTED_EDGE ( 'NONE', *, *, #1800, .F. ) ;
#1815 = AXIS2_PLACEMENT_3D ( 'NONE', #5134, #10, #6749 ) ;
#1816 = EDGE_CURVE ( 'NONE', #478, #2671, #4506, .T. ) ;
#1817 = CARTESIAN_POINT ( 'NONE',  ( 303.3333333333333144, -14.99999999999999822, 162.5000000000000853 ) ) ;
#1818 = FACE_OUTER_BOUND ( 'NONE', #7321, .T. ) ;
#1819 = DIRECTION ( 'NONE',  ( 0.000000000000000000, 0.000000000000000000, -1.000000000000000000 ) ) ;
#1820 = CARTESIAN_POINT ( 'NONE',  ( 155.0000000000000000, 8.660254037844390851, 145.0000000000000284 ) ) ;
#1821 = SURFACE_SIDE_STYLE ('',( #5958 ) ) ;
#1822 = ORIENTED_EDGE ( 'NONE', *, *, #368, .F. ) ;
#1823 = EDGE_CURVE ( 'NONE', #3661, #5128, #4733, .T. ) ;
#1824 = DIRECTION ( 'NONE',  ( 6.123233995736766036E-17, -1.000000000000000000, 0.000000000000000000 ) ) ;
#1825 = PLANE ( 'NONE',  #1827 ) ;
#1826 = AXIS2_PLACEMENT_3D ( 'NONE', #3823, #2768, #4429 ) ;
#1827 = AXIS2_PLACEMENT_3D ( 'NONE', #2939, #3660, #5880 ) ;
#1828 = UNCERTAINTY_MEASURE_WITH_UNIT (LENGTH_MEASURE( 1.000000000000000082E-05 ), #2358, 'distance_accuracy_value', 'NONE');
#1829 = ORIENTED_EDGE ( 'NONE', *, *, #4389, .F. ) ;
#1830 = ORIENTED_EDGE ( 'NONE', *, *, #6194, .F. ) ;
#1831 = CARTESIAN_POINT ( 'NONE',  ( 195.0000000000000000, -8.660254037844389075, 140.0000000000000000 ) ) ;
#1832 = CARTESIAN_POINT ( 'NONE',  ( -3.436319922987618902, 2.634841920961291439, -3.531542292955721862 ) ) ;
#1833 = AXIS2_PLACEMENT_3D ( 'NONE', #4520, #6809, #6240 ) ;
#1834 = COLOUR_RGB ( '',1.000000000000000000, 0.9490196078431372140, 0.9098039215686274384 ) ;
#1835 = CARTESIAN_POINT ( 'NONE',  ( 3.999999999999999112, 2.309401076758497595, -3.504271511726784194 ) ) ;
#1836 = CARTESIAN_POINT ( 'NONE',  ( 1.734723475976807094E-15, 4.618802153517012954, -0.4999999999999995559 ) ) ;
#1837 = CARTESIAN_POINT ( 'NONE',  ( 235.0000000000000000, -8.660254037844389075, 139.9990000000000236 ) ) ;
#1838 = VECTOR ( 'NONE', #341, 1000.000000000000000 ) ;
#1839 = STYLED_ITEM ( 'NONE', ( #5878 ), #4767 ) ;
#1840 = EDGE_CURVE ( 'NONE', #5914, #2630, #6783, .T. ) ;
#1841 = ORIENTED_EDGE ( 'NONE', *, *, #2351, .T. ) ;
#1842 = ORIENTED_EDGE ( 'NONE', *, *, #7244, .F. ) ;
#1843 = DIRECTION ( 'NONE',  ( 0.000000000000000000, 0.000000000000000000, -1.000000000000000000 ) ) ;
#1844 = ORIENTED_EDGE ( 'NONE', *, *, #474, .T. ) ;
#1845 = AXIS2_PLACEMENT_3D ( 'NONE', #4035, #706, #5800 ) ;
#1846 =( LENGTH_UNIT ( ) NAMED_UNIT ( * ) SI_UNIT ( .MILLI., .METRE. ) );
#1847 = AXIS2_PLACEMENT_3D ( 'NONE', #554, #3871, #7250 ) ;
#1848 = CARTESIAN_POINT ( 'NONE',  ( -4.197312064133472020, -0.8182229787990021874, -3.502518405183886685 ) ) ;
#1849 = ORIENTED_EDGE ( 'NONE', *, *, #1263, .T. ) ;
#1850 = VECTOR ( 'NONE', #5715, 1000.000000000000114 ) ;
#1851 = CARTESIAN_POINT ( 'NONE',  ( 124.9999999999999858, 8.660254037844390851, 139.9990000000000236 ) ) ;
#1852 = ADVANCED_FACE ( 'NONE', ( #6717 ), #4243, .F. ) ;
#1853 = CIRCLE ( 'NONE', #6304, 2.500000000000000444 ) ;
#1854 = DIRECTION ( 'NONE',  ( -0.000000000000000000, -0.000000000000000000, 1.000000000000000000 ) ) ;
#1855 = DIRECTION ( 'NONE',  ( 0.000000000000000000, 0.000000000000000000, -1.000000000000000000 ) ) ;
#1856 = ORIENTED_EDGE ( 'NONE', *, *, #6926, .F. ) ;
#1857 = DIRECTION ( 'NONE',  ( 0.000000000000000000, 0.000000000000000000, -1.000000000000000000 ) ) ;
#1858 = COLOUR_RGB ( '',1.000000000000000000, 0.9490196078431372140, 0.9098039215686274384 ) ;
#1859 = DIRECTION ( 'NONE',  ( -0.000000000000000000, 1.000000000000000000, -0.000000000000000000 ) ) ;
#1860 = DIRECTION ( 'NONE',  ( -0.000000000000000000, -1.000000000000000000, -0.000000000000000000 ) ) ;
#1861 = SHAPE_REPRESENTATION_RELATIONSHIP ( 'NONE' , 'NONE' ,  #5023, #4767 ) ;
#1862 = ORIENTED_EDGE ( 'NONE', *, *, #6060, .T. ) ;
#1863 = DIRECTION ( 'NONE',  ( -1.000000000000000000, -0.000000000000000000, -0.000000000000000000 ) ) ;
#1864 = EDGE_CURVE ( 'NONE', #7332, #4123, #7277, .T. ) ;
#1865 = ORIENTED_EDGE ( 'NONE', *, *, #2024, .F. ) ;
#1866 = ORIENTED_EDGE ( 'NONE', *, *, #3370, .F. ) ;
#1867 = CARTESIAN_POINT ( 'NONE',  ( 4.000000000000000000, 2.309401076758497151, -3.433295621305379353 ) ) ;
#1868 = DIRECTION ( 'NONE',  ( -1.000000000000000000, -0.000000000000000000, -0.000000000000000000 ) ) ;
#1869 = CARTESIAN_POINT ( 'NONE',  ( 164.9999999999999716, 8.660254037844390851, 140.0000000000000000 ) ) ;
#1870 = DIRECTION ( 'NONE',  ( 0.000000000000000000, 0.000000000000000000, -1.000000000000000000 ) ) ;
#1871 = CARTESIAN_POINT ( 'NONE',  ( 386.6666666666666288, -25.00000000000000000, 159.8500000000001080 ) ) ;
#1872 = EDGE_CURVE ( 'NONE', #932, #1873, #2097, .T. ) ;
#1873 = VERTEX_POINT ( 'NONE', #3860 ) ;
#1874 = ORIENTED_EDGE ( 'NONE', *, *, #6455, .F. ) ;
#1875 = EDGE_CURVE ( 'NONE', #6108, #4203, #1048, .T. ) ;
#1876 = DIRECTION ( 'NONE',  ( 0.000000000000000000, 0.000000000000000000, -1.000000000000000000 ) ) ;
#1877 = EDGE_LOOP ( 'NONE', ( #3340, #747, #5135, #1756 ) ) ;
#1878 = PRODUCT_RELATED_PRODUCT_CATEGORY ( 'part', '', ( #5289 ) ) ;
#1879 = CARTESIAN_POINT ( 'NONE',  ( -4.203934362469166963, -1.640673743454851286, -3.598432614606932756 ) ) ;
#1880 = ORIENTED_EDGE ( 'NONE', *, *, #6777, .F. ) ;
#1881 = CARTESIAN_POINT ( 'NONE',  ( 164.9999999999999716, 8.660254037844390851, 140.0000000000000000 ) ) ;
#1882 = ORIENTED_EDGE ( 'NONE', *, *, #4305, .F. ) ;
#1883 = CARTESIAN_POINT ( 'NONE',  ( 136.6666666666666288, -20.00000000000000000, 165.1500000000000625 ) ) ;
#1884 = VERTEX_POINT ( 'NONE', #4463 ) ;
#1885 = EDGE_CURVE ( 'NONE', #1000, #1976, #4456, .T. ) ;
#1886 = DIRECTION ( 'NONE',  ( 1.000000000000000000, 0.000000000000000000, 0.000000000000000000 ) ) ;
#1887 = DIRECTION ( 'NONE',  ( 1.000000000000000000, 0.000000000000000000, 0.000000000000000000 ) ) ;
#1888 = DIRECTION ( 'NONE',  ( 1.000000000000000000, 0.000000000000000000, 0.000000000000000000 ) ) ;
#1889 = DIRECTION ( 'NONE',  ( 0.000000000000000000, 0.000000000000000000, 1.000000000000000000 ) ) ;
#1890 = EDGE_LOOP ( 'NONE', ( #1789, #7069, #4617, #1035 ) ) ;
#1891 = LINE ( 'NONE', #6377, #4105 ) ;
#1892 = ORIENTED_EDGE ( 'NONE', *, *, #652, .T. ) ;
#1893 = EDGE_LOOP ( 'NONE', ( #5939, #5620, #4167, #1439 ) ) ;
#1894 =( REPRESENTATION_RELATIONSHIP ('NONE','NONE', #5587, #1193 ) REPRESENTATION_RELATIONSHIP_WITH_TRANSFORMATION ( #1544 )SHAPE_REPRESENTATION_RELATIONSHIP( ) );
#1895 = CARTESIAN_POINT ( 'NONE',  ( 303.3333333333333144, -20.00000000000000000, 159.8500000000001080 ) ) ;
#1896 = CARTESIAN_POINT ( 'NONE',  ( -2.756197834950067094, -3.027510591568735254, -3.223146290109809797 ) ) ;
#1897 = CARTESIAN_POINT ( 'NONE',  ( -1.999999999999998224, 0.000000000000000000, 0.000000000000000000 ) ) ;
#1898 = DIRECTION ( 'NONE',  ( -0.000000000000000000, -1.000000000000000000, -0.000000000000000000 ) ) ;
#1899 = ADVANCED_FACE ( 'NONE', ( #1507 ), #3288, .F. ) ;
#1900 = CIRCLE ( 'NONE', #6115, 2.649999999999985700 ) ;
#1901 = EDGE_CURVE ( 'NONE', #2671, #2792, #5213, .T. ) ;
#1902 = CARTESIAN_POINT ( 'NONE',  ( -4.000000000000000000, -2.309401076758515803, -0.4999999999999995559 ) ) ;
#1903 = CARTESIAN_POINT ( 'NONE',  ( 24.55500000000002103, 0.000000000000000000, 2.500000000000001332 ) ) ;
#1904 = VERTEX_POINT ( 'NONE', #5622 ) ;
#1905 = CONTEXT_DEPENDENT_SHAPE_REPRESENTATION ( #4108, #698 ) ;
#1906 = DIRECTION ( 'NONE',  ( -0.000000000000000000, -0.000000000000000000, -1.000000000000000000 ) ) ;
#1907 = EDGE_LOOP ( 'NONE', ( #2895, #322, #5015, #3092 ) ) ;
#1908 = ADVANCED_FACE ( 'NONE', ( #5588 ), #1617, .F. ) ;
#1909 = PRODUCT_DEFINITION_SHAPE ( 'NONE', 'NONE',  #7388 ) ;
#1910 = CARTESIAN_POINT ( 'NONE',  ( -4.000000000000000000, 2.471528634177585282, -3.686887442155186712 ) ) ;
#1911 = ORIENTED_EDGE ( 'NONE', *, *, #6967, .T. ) ;
#1912 = ORIENTED_EDGE ( 'NONE', *, *, #1423, .F. ) ;
#1913 = CARTESIAN_POINT ( 'NONE',  ( 2.500000000000000000, 0.000000000000000000, 0.000000000000000000 ) ) ;
#1914 = CARTESIAN_POINT ( 'NONE',  ( -30.00000000000002842, -25.00000000000000000, 200.0000000000000000 ) ) ;
#1915 = AXIS2_PLACEMENT_3D ( 'NONE', #2600, #4262, #4858 ) ;
#1916 = ORIENTED_EDGE ( 'NONE', *, *, #5184, .F. ) ;
#1917 = CARTESIAN_POINT ( 'NONE',  ( 53.33333333333330017, -20.00000000000000000, 165.1500000000000625 ) ) ;
#1918 = ORIENTED_EDGE ( 'NONE', *, *, #4537, .F. ) ;
#1919 = EDGE_CURVE ( 'NONE', #5019, #3377, #675, .T. ) ;
#1920 = AXIS2_PLACEMENT_3D ( 'NONE', #6002, #5549, #2011 ) ;
#1921 = CARTESIAN_POINT ( 'NONE',  ( 4.000000000001088907, 1.658577278524410170, -3.531553309554541720 ) ) ;
#1922 = ITEM_DEFINED_TRANSFORMATION ( 'NONE', 'NONE', #6627,  #1963 ) ;
#1923 = DIRECTION ( 'NONE',  ( 0.000000000000000000, 0.000000000000000000, 1.000000000000000000 ) ) ;
#1924 = DIRECTION ( 'NONE',  ( -1.000000000000000000, -0.000000000000000000, -0.000000000000000000 ) ) ;
#1925 = EDGE_CURVE ( 'NONE', #6714, #1367, #6083, .T. ) ;
#1926 =( LENGTH_UNIT ( ) NAMED_UNIT ( * ) SI_UNIT ( .MILLI., .METRE. ) );
#1927 = ORIENTED_EDGE ( 'NONE', *, *, #5201, .F. ) ;
#1928 = DIRECTION ( 'NONE',  ( -1.000000000000000000, -0.000000000000000000, -0.000000000000000000 ) ) ;
#1929 = PRODUCT_DEFINITION_SHAPE ( 'NONE', 'NONE',  #2657 ) ;
#1930 = AXIS2_PLACEMENT_3D ( 'NONE', #5601, #3258, #1556 ) ;
#1931 = CLOSED_SHELL ( 'NONE', ( #4973, #2450, #5528, #2325, #5277, #4629, #2928, #3996, #6463, #6591, #1549, #1699, #2441, #5052, #3178, #6010, #5335, #1677, #878, #4901, #4099, #370, #3043, #7043, #1908, #3932, #5821 ) ) ;
#1932 = VERTEX_POINT ( 'NONE', #3940 ) ;
#1933 = VERTEX_POINT ( 'NONE', #945 ) ;
#1934 = PLANE ( 'NONE',  #142 ) ;
#1935 = FACE_OUTER_BOUND ( 'NONE', #4057, .T. ) ;
#1936 = CARTESIAN_POINT ( 'NONE',  ( 2.500000000000000000, 2.357898499370433054, -1.951563910473907981E-15 ) ) ;
#1937 = CARTESIAN_POINT ( 'NONE',  ( 1.799999999999996048, 1.249139735130300365E-15, 10.20000000000000107 ) ) ;
#1938 = B_SPLINE_CURVE_WITH_KNOTS ( 'NONE', 3,
 ( #6690, #6092, #3707, #2660, #3171, #1037 ),
 .UNSPECIFIED., .F., .F.,
 ( 4, 2, 4 ),
 ( 0.002365888236227995517, 0.003551327329835084114, 0.004736766423442172712 ),
 .UNSPECIFIED. ) ;
#1939 = VECTOR ( 'NONE', #5291, 1000.000000000000000 ) ;
#1940 = CARTESIAN_POINT ( 'NONE',  ( 0.000000000000000000, 0.000000000000000000, 0.000000000000000000 ) ) ;
#1941 = ADVANCED_FACE ( 'NONE', ( #2805 ), #7195, .F. ) ;
#1942 = CARTESIAN_POINT ( 'NONE',  ( 365.0000000000000000, -8.660254037844389075, 139.9990000000000236 ) ) ;
#1943 = APPLICATION_CONTEXT ( 'automotive_design' ) ;
#1944 = EDGE_CURVE ( 'NONE', #2273, #853, #4540, .T. ) ;
#1945 = ORIENTED_EDGE ( 'NONE', *, *, #5712, .F. ) ;
#1946 = CIRCLE ( 'NONE', #5557, 10.20000000000000107 ) ;
#1947 = CONTEXT_DEPENDENT_SHAPE_REPRESENTATION ( #6421, #6619 ) ;
#1948 = LINE ( 'NONE', #1361, #3023 ) ;
#1949 = VERTEX_POINT ( 'NONE', #5705 ) ;
#1950 =( NAMED_UNIT ( * ) PLANE_ANGLE_UNIT ( ) SI_UNIT ( $, .RADIAN. ) );
#1951 = FILL_AREA_STYLE ('',( #2546 ) ) ;
#1952 = VECTOR ( 'NONE', #5276, 1000.000000000000000 ) ;
#1953 = MECHANICAL_DESIGN_GEOMETRIC_PRESENTATION_REPRESENTATION (  '', ( #3392 ), #4358 ) ;
#1954 = CARTESIAN_POINT ( 'NONE',  ( -20.63749999999999929, 0.000000000000000000, -11.05000000000000071 ) ) ;
#1955 = EDGE_CURVE ( 'NONE', #1344, #6275, #2443, .T. ) ;
#1956 = ORIENTED_EDGE ( 'NONE', *, *, #6241, .T. ) ;
#1957 = VECTOR ( 'NONE', #464, 1000.000000000000000 ) ;
#1958 = ORIENTED_EDGE ( 'NONE', *, *, #104, .T. ) ;
#1959 = DIRECTION ( 'NONE',  ( 0.000000000000000000, 0.000000000000000000, -1.000000000000000000 ) ) ;
#1960 = DIRECTION ( 'NONE',  ( 1.224646799147353207E-16, 1.000000000000000000, 0.000000000000000000 ) ) ;
#1961 = ORIENTED_EDGE ( 'NONE', *, *, #5344, .T. ) ;
#1962 = B_SPLINE_CURVE_WITH_KNOTS ( 'NONE', 3,
 ( #3627, #5356, #3163, #3664, #5463, #351, #2494, #7084 ),
 .UNSPECIFIED., .F., .F.,
 ( 4, 2, 2, 4 ),
 ( 0.005725059856848645212, 0.006314084072593634418, 0.006903108288338624492, 0.008081156719828603771 ),
 .UNSPECIFIED. ) ;
#1963 = AXIS2_PLACEMENT_3D ( 'NONE', #2294, #628, #5829 ) ;
#1964 = EDGE_CURVE ( 'NONE', #1538, #767, #6370, .T. ) ;
#1965 = AXIS2_PLACEMENT_3D ( 'NONE', #588, #5246, #6423 ) ;
#1966 = ORIENTED_EDGE ( 'NONE', *, *, #2368, .F. ) ;
#1967 = CARTESIAN_POINT ( 'NONE',  ( 4.000000000000000888, -0.8578082829538523635, -3.433262215449808696 ) ) ;
#1968 = ITEM_DEFINED_TRANSFORMATION ( 'NONE', 'NONE', #2187,  #1963 ) ;
#1969 = CARTESIAN_POINT ( 'NONE',  ( -30.00000000000002842, -20.00000000000000000, 180.0000000000000284 ) ) ;
#1970 = CYLINDRICAL_SURFACE ( 'NONE', #2320, 2.649999999999985700 ) ;
#1971 = AXIS2_PLACEMENT_3D ( 'NONE', #2233, #6461, #1843 ) ;
#1972 = VERTEX_POINT ( 'NONE', #6831 ) ;
#1973 = FACE_BOUND ( 'NONE', #5709, .T. ) ;
#1974 = EDGE_LOOP ( 'NONE', ( #5699, #7205, #5381, #687 ) ) ;
#1975 = AXIS2_PLACEMENT_3D ( 'NONE', #1192, #4098, #4633 ) ;
#1976 = VERTEX_POINT ( 'NONE', #580 ) ;
#1977 = PLANE ( 'NONE',  #1088 ) ;
#1978 = DIRECTION ( 'NONE',  ( 0.000000000000000000, -1.224646799147352468E-16, 1.000000000000000000 ) ) ;
#1979 = DIRECTION ( 'NONE',  ( 1.000000000000000000, 0.000000000000000000, 0.000000000000000000 ) ) ;
#1980 = DIRECTION ( 'NONE',  ( 0.000000000000000000, 1.000000000000000000, 0.000000000000000000 ) ) ;
#1981 = CARTESIAN_POINT ( 'NONE',  ( 2.500000000000000000, -2.357898499370432610, 3.252606517456513302E-15 ) ) ;
#1982 = CARTESIAN_POINT ( 'NONE',  ( 386.6666666666666288, -25.00000000000000000, 165.1500000000000625 ) ) ;
#1983 =( GEOMETRIC_REPRESENTATION_CONTEXT ( 3 ) GLOBAL_UNCERTAINTY_ASSIGNED_CONTEXT ( ( #718 ) ) GLOBAL_UNIT_ASSIGNED_CONTEXT ( ( #3530, #5599, #5042 ) ) REPRESENTATION_CONTEXT ( 'NONE', 'WORKASPACE' ) );
#1984 = ORIENTED_EDGE ( 'NONE', *, *, #1590, .F. ) ;
#1985 = LINE ( 'NONE', #4024, #5867 ) ;
#1986 = CARTESIAN_POINT ( 'NONE',  ( -30.00000000000002842, 15.00000000000000000, 145.0000000000000284 ) ) ;
#1987 = VERTEX_POINT ( 'NONE', #4676 ) ;
#1988 = ADVANCED_FACE ( 'NONE', ( #934 ), #5169, .F. ) ;
#1989 = DIRECTION ( 'NONE',  ( 1.000000000000000000, 0.000000000000000000, -0.000000000000000000 ) ) ;
#1990 = ORIENTED_EDGE ( 'NONE', *, *, #1240, .T. ) ;
#1991 = ORIENTED_EDGE ( 'NONE', *, *, #2112, .F. ) ;
#1992 = CARTESIAN_POINT ( 'NONE',  ( 1.799999999999996048, 0.000000000000000000, 0.000000000000000000 ) ) ;
#1993 = ADVANCED_FACE ( 'NONE', ( #5238, #711 ), #2836, .T. ) ;
#1994 = CARTESIAN_POINT ( 'NONE',  ( 4.999999999999999112, -8.660254037844389075, -150.0000000000000000 ) ) ;
#1995 = EDGE_CURVE ( 'NONE', #5227, #6735, #2563, .T. ) ;
#1996 = PLANE ( 'NONE',  #2421 ) ;
#1997 = CARTESIAN_POINT ( 'NONE',  ( 0.2277608394786177770, 0.000000000000000000, 10.72500000000000142 ) ) ;
#1998 =( REPRESENTATION_RELATIONSHIP ('NONE','NONE', #5587, #6025 ) REPRESENTATION_RELATIONSHIP_WITH_TRANSFORMATION ( #2311 )SHAPE_REPRESENTATION_RELATIONSHIP( ) );
#1999 = ORIENTED_EDGE ( 'NONE', *, *, #6583, .F. ) ;
#2000 = DIRECTION ( 'NONE',  ( 0.000000000000000000, 0.000000000000000000, -1.000000000000000000 ) ) ;
#2001 = DIRECTION ( 'NONE',  ( -0.000000000000000000, -0.000000000000000000, 1.000000000000000000 ) ) ;
#2002 = DIRECTION ( 'NONE',  ( 1.000000000000000000, 0.000000000000000000, 0.000000000000000000 ) ) ;
#2003 = EDGE_CURVE ( 'NONE', #84, #4019, #3503, .T. ) ;
#2004 = DIRECTION ( 'NONE',  ( 0.000000000000000000, 0.000000000000000000, 1.000000000000000000 ) ) ;
#2005 = ORIENTED_EDGE ( 'NONE', *, *, #5644, .T. ) ;
#2006 = CARTESIAN_POINT ( 'NONE',  ( 1.411581201560190495E-15, 4.862606272033091592, -3.745885042887436622 ) ) ;
#2007 = VERTEX_POINT ( 'NONE', #1724 ) ;
#2008 = ORIENTED_EDGE ( 'NONE', *, *, #5138, .T. ) ;
#2009 = FACE_OUTER_BOUND ( 'NONE', #4385, .T. ) ;
#2010 = CARTESIAN_POINT ( 'NONE',  ( 303.3333333333333144, -20.00000000000000000, -162.5000000000000853 ) ) ;
#2011 = DIRECTION ( 'NONE',  ( 0.000000000000000000, -0.000000000000000000, -1.000000000000000000 ) ) ;
#2012 = FACE_OUTER_BOUND ( 'NONE', #6212, .T. ) ;
#2013 = CARTESIAN_POINT ( 'NONE',  ( 0.000000000000000000, -2.357898499370432610, 3.252606517456513302E-15 ) ) ;
#2014 = FACE_OUTER_BOUND ( 'NONE', #5398, .T. ) ;
#2015 = ORIENTED_EDGE ( 'NONE', *, *, #6750, .T. ) ;
#2016 = DIRECTION ( 'NONE',  ( 1.000000000000000000, 0.000000000000000000, -0.000000000000000000 ) ) ;
#2017 = DIRECTION ( 'NONE',  ( -1.000000000000000000, -0.000000000000000000, -0.000000000000000000 ) ) ;
#2018 = VERTEX_POINT ( 'NONE', #6933 ) ;
#2019 = DIRECTION ( 'NONE',  ( -1.000000000000000000, -0.000000000000000000, -0.000000000000000000 ) ) ;
#2020 = AXIS2_PLACEMENT_3D ( 'NONE', #2835, #4539, #2309 ) ;
#2021 =( LENGTH_UNIT ( ) NAMED_UNIT ( * ) SI_UNIT ( .MILLI., .METRE. ) );
#2022 = CARTESIAN_POINT ( 'NONE',  ( 45.00000000000000000, 8.660254037844390851, 140.0000000000000000 ) ) ;
#2023 = DIRECTION ( 'NONE',  ( 1.000000000000000000, 0.000000000000000000, 0.000000000000000000 ) ) ;
#2024 = EDGE_CURVE ( 'NONE', #2259, #6322, #4041, .T. ) ;
#2025 = CIRCLE ( 'NONE', #1092, 2.500000000000000888 ) ;
#2026 = ORIENTED_EDGE ( 'NONE', *, *, #2351, .F. ) ;
#2027 = DIRECTION ( 'NONE',  ( 0.000000000000000000, 0.000000000000000000, 1.000000000000000000 ) ) ;
#2028 = VERTEX_POINT ( 'NONE', #2310 ) ;
#2029 = PLANE ( 'NONE',  #6297 ) ;
#2030 = CIRCLE ( 'NONE', #6477, 2.041999999999999815 ) ;
#2031 = CARTESIAN_POINT ( 'NONE',  ( -4.211140560182196957, 2.431303136016537803, -3.745885042887433514 ) ) ;
#2032 = DIRECTION ( 'NONE',  ( -0.000000000000000000, 1.000000000000000000, -0.000000000000000000 ) ) ;
#2033 = EDGE_CURVE ( 'NONE', #719, #214, #1853, .T. ) ;
#2034 = EDGE_LOOP ( 'NONE', ( #875, #1722, #21, #4239 ) ) ;
#2035 = ADVANCED_FACE ( 'NONE', ( #1818 ), #6066, .F. ) ;
#2036 = VECTOR ( 'NONE', #2001, 1000.000000000000000 ) ;
#2037 = DIRECTION ( 'NONE',  ( 0.000000000000000000, 0.000000000000000000, -1.000000000000000000 ) ) ;
#2038 = ITEM_DEFINED_TRANSFORMATION ( 'NONE', 'NONE', #4102,  #1963 ) ;
#2039 = CARTESIAN_POINT ( 'NONE',  ( 435.0000000000000568, 8.660254037844390851, 139.9990000000000236 ) ) ;
#2040 = CARTESIAN_POINT ( 'NONE',  ( 53.33333333333330017, -20.00000000000000000, 162.5000000000000853 ) ) ;
#2041 = DIRECTION ( 'NONE',  ( 1.000000000000000000, 6.123233995736766036E-17, -6.123233995736764803E-17 ) ) ;
#2042 = ORIENTED_EDGE ( 'NONE', *, *, #184, .F. ) ;
#2043 = CARTESIAN_POINT ( 'NONE',  ( 205.0000000000000284, 8.660254037844390851, 140.0000000000000000 ) ) ;
#2044 = VECTOR ( 'NONE', #3739, 1000.000000000000000 ) ;
#2045 = VECTOR ( 'NONE', #6550, 1000.000000000000000 ) ;
#2046 = EDGE_CURVE ( 'NONE', #647, #7294, #1271, .T. ) ;
#2047 = ORIENTED_EDGE ( 'NONE', *, *, #3451, .T. ) ;
#2048 = EDGE_LOOP ( 'NONE', ( #4568, #1849, #5404, #4524, #1500 ) ) ;
#2049 = LINE ( 'NONE', #2095, #2266 ) ;
#2050 = CARTESIAN_POINT ( 'NONE',  ( 4.140404888673277384, 2.228338276487440428, -3.686887068327033390 ) ) ;
#2051 = DIRECTION ( 'NONE',  ( -0.000000000000000000, 1.000000000000000000, -0.000000000000000000 ) ) ;
#2052 = FACE_OUTER_BOUND ( 'NONE', #2116, .T. ) ;
#2053 = AXIS2_PLACEMENT_3D ( 'NONE', #162, #93, #6415 ) ;
#2054 = PLANE ( 'NONE',  #412 ) ;
#2055 = CARTESIAN_POINT ( 'NONE',  ( 0.000000000000000000, 0.000000000000000000, 0.000000000000000000 ) ) ;
#2056 = DIRECTION ( 'NONE',  ( 0.000000000000000000, 0.000000000000000000, 1.000000000000000000 ) ) ;
#2057 = EDGE_CURVE ( 'NONE', #5128, #6618, #1687, .T. ) ;
#2058 = EDGE_LOOP ( 'NONE', ( #5443, #81, #6928 ) ) ;
#2059 = PRODUCT_DEFINITION_SHAPE ( 'NONE', 'NONE',  #7355 ) ;
#2060 = CARTESIAN_POINT ( 'NONE',  ( -30.00000000000002842, -20.00000000000000000, 200.0000000000000000 ) ) ;
#2061 = AXIS2_PLACEMENT_3D ( 'NONE', #306, #5534, #3157 ) ;
#2062 = VERTEX_POINT ( 'NONE', #16 ) ;
#2063 = TOROIDAL_SURFACE ( 'NONE', #5413, 13.29999999999999893, 0.2000000000000027034 ) ;
#2064 = SURFACE_SIDE_STYLE ('',( #7289 ) ) ;
#2065 = TOROIDAL_SURFACE ( 'NONE', #171, 2.700000000000001066, 0.2000000000000000111 ) ;
#2066 = SURFACE_STYLE_USAGE ( .BOTH. , #4245 ) ;
#2067 = CARTESIAN_POINT ( 'NONE',  ( 395.0000000000000000, 8.660254037844390851, 139.9990000000000236 ) ) ;
#2068 = EDGE_CURVE ( 'NONE', #5338, #4282, #6898, .T. ) ;
#2069 = CONTEXT_DEPENDENT_SHAPE_REPRESENTATION ( #4204, #5214 ) ;
#2070 = DIRECTION ( 'NONE',  ( 0.000000000000000000, 0.000000000000000000, -1.000000000000000000 ) ) ;
#2071 = VECTOR ( 'NONE', #2769, 1000.000000000000000 ) ;
#2072 = VERTEX_POINT ( 'NONE', #610 ) ;
#2073 = DIRECTION ( 'NONE',  ( 0.000000000000000000, 0.000000000000000000, 1.000000000000000000 ) ) ;
#2074 = EDGE_LOOP ( 'NONE', ( #6542, #4949, #5458, #606 ) ) ;
#2075 = CIRCLE ( 'NONE', #6508, 2.649999999999985700 ) ;
#2076 = DIRECTION ( 'NONE',  ( -1.000000000000000000, 0.000000000000000000, 0.000000000000000000 ) ) ;
#2077 = CIRCLE ( 'NONE', #4596, 2.649999999999985700 ) ;
#2078 = DIRECTION ( 'NONE',  ( 0.000000000000000000, 0.000000000000000000, 1.000000000000000000 ) ) ;
#2079 = SURFACE_STYLE_USAGE ( .BOTH. , #931 ) ;
#2080 = UNCERTAINTY_MEASURE_WITH_UNIT (LENGTH_MEASURE( 1.000000000000000082E-05 ), #4291, 'distance_accuracy_value', 'NONE');
#2081 = EDGE_LOOP ( 'NONE', ( #1750, #4190 ) ) ;
#2082 = AXIS2_PLACEMENT_3D ( 'NONE', #7042, #1889, #1339 ) ;
#2083 = B_SPLINE_CURVE_WITH_KNOTS ( 'NONE', 3,
 ( #6546, #1409, #6620, #3682, #843, #3718 ),
 .UNSPECIFIED., .F., .F.,
 ( 4, 2, 4 ),
 ( -3.640115492409406142E-06, 0.0002066546034006526487, 0.0004169493222937146744 ),
 .UNSPECIFIED. ) ;
#2084 = CARTESIAN_POINT ( 'NONE',  ( 195.0000000000000000, 8.660254037844390851, 139.9990000000000236 ) ) ;
#2085 = ADVANCED_FACE ( 'NONE', ( #4572 ), #6865, .F. ) ;
#2086 = DIRECTION ( 'NONE',  ( 0.000000000000000000, -1.000000000000000000, 0.000000000000000000 ) ) ;
#2087 = DIRECTION ( 'NONE',  ( -1.000000000000000000, 0.000000000000000000, -0.000000000000000000 ) ) ;
#2088 = CIRCLE ( 'NONE', #1739, 9.999999999999998224 ) ;
#2089 = CARTESIAN_POINT ( 'NONE',  ( 219.9999999999999716, -30.00000000000000355, 162.5000000000000853 ) ) ;
#2090 = CIRCLE ( 'NONE', #672, 2.649999999999985700 ) ;
#2091 = EDGE_LOOP ( 'NONE', ( #5202, #2859, #2616, #7285 ) ) ;
#2092 = FACE_BOUND ( 'NONE', #2505, .T. ) ;
#2093 = ORIENTED_EDGE ( 'NONE', *, *, #6554, .T. ) ;
#2094 = ORIENTED_EDGE ( 'NONE', *, *, #1518, .F. ) ;
#2095 = CARTESIAN_POINT ( 'NONE',  ( 395.0000000000000000, -8.660254037844389075, 145.0000000000000284 ) ) ;
#2096 = AXIS2_PLACEMENT_3D ( 'NONE', #4829, #6529, #1425 ) ;
#2097 = LINE ( 'NONE', #2134, #3644 ) ;
#2098 = ITEM_DEFINED_TRANSFORMATION ( 'NONE', 'NONE', #1492,  #1963 ) ;
#2099 = CARTESIAN_POINT ( 'NONE',  ( 4.999999999999999112, 8.660254037844390851, 139.9990000000000236 ) ) ;
#2100 = CYLINDRICAL_SURFACE ( 'NONE', #6885, 11.05000000000000071 ) ;
#2101 = EDGE_CURVE ( 'NONE', #7234, #1078, #644, .T. ) ;
#2102 = DIRECTION ( 'NONE',  ( 1.000000000000000000, 0.000000000000000000, 0.000000000000000000 ) ) ;
#2103 = DIRECTION ( 'NONE',  ( -1.000000000000000000, -0.000000000000000000, -0.000000000000000000 ) ) ;
#2104 = EDGE_CURVE ( 'NONE', #2352, #2399, #3287, .T. ) ;
#2105 = AXIS2_PLACEMENT_3D ( 'NONE', #4891, #2032, #258 ) ;
#2106 = EDGE_LOOP ( 'NONE', ( #6829, #534, #1276, #4886 ) ) ;
#2107 = CARTESIAN_POINT ( 'NONE',  ( 2.000000000000001776, 0.000000000000000000, -12.44999999999999929 ) ) ;
#2108 = CARTESIAN_POINT ( 'NONE',  ( 45.00000000000000000, -8.660254037844389075, 145.0000000000000284 ) ) ;
#2109 = CARTESIAN_POINT ( 'NONE',  ( 435.0000000000000568, 8.660254037844390851, 145.0000000000000284 ) ) ;
#2110 = PRESENTATION_STYLE_ASSIGNMENT (( #7252 ) ) ;
#2111 = CIRCLE ( 'NONE', #1519, 10.20000000000000107 ) ;
#2112 = EDGE_CURVE ( 'NONE', #7144, #5826, #2965, .T. ) ;
#2113 = DIRECTION ( 'NONE',  ( -0.000000000000000000, 1.000000000000000000, -0.000000000000000000 ) ) ;
#2114 = CARTESIAN_POINT ( 'NONE',  ( 435.0000000000000568, 8.660254037844390851, 145.0000000000000284 ) ) ;
#2115 = EDGE_LOOP ( 'NONE', ( #6569, #2579, #4972 ) ) ;
#2116 = EDGE_LOOP ( 'NONE', ( #6231, #3523, #3692, #7111 ) ) ;
#2117 = DIRECTION ( 'NONE',  ( 0.000000000000000000, 0.000000000000000000, 1.000000000000000000 ) ) ;
#2118 = EDGE_LOOP ( 'NONE', ( #3607, #6919, #1485, #6157 ) ) ;
#2119 = CARTESIAN_POINT ( 'NONE',  ( 355.0000000000000000, -8.660254037844389075, 139.9990000000000236 ) ) ;
#2120 = CARTESIAN_POINT ( 'NONE',  ( -1.799999999999996048, 0.000000000000000000, 0.000000000000000000 ) ) ;
#2121 = CARTESIAN_POINT ( 'NONE',  ( 435.0000000000000568, 8.660254037844390851, 140.0000000000000000 ) ) ;
#2122 = ORIENTED_EDGE ( 'NONE', *, *, #1493, .F. ) ;
#2123 = LINE ( 'NONE', #8, #6736 ) ;
#2124 = CARTESIAN_POINT ( 'NONE',  ( -5.000000000000000888, 8.660254037844390851, 150.0000000000000000 ) ) ;
#2125 = LINE ( 'NONE', #6585, #5517 ) ;
#2126 = DIRECTION ( 'NONE',  ( 0.000000000000000000, 0.000000000000000000, -1.000000000000000000 ) ) ;
#2127 = CARTESIAN_POINT ( 'NONE',  ( 136.6666666666666288, -10.00000000000000000, 162.5000000000000853 ) ) ;
#2128 = ORIENTED_EDGE ( 'NONE', *, *, #958, .F. ) ;
#2129 = CARTESIAN_POINT ( 'NONE',  ( -1.799999999999996048, 0.000000000000000000, -10.20000000000000107 ) ) ;
#2130 = ADVANCED_FACE ( 'NONE', ( #2413 ), #5897, .F. ) ;
#2131 = ORIENTED_EDGE ( 'NONE', *, *, #3639, .F. ) ;
#2132 = EDGE_LOOP ( 'NONE', ( #578, #5329, #6288, #6562 ) ) ;
#2133 = CARTESIAN_POINT ( 'NONE',  ( 2.500000000000000000, 0.000000000000000000, 0.000000000000000000 ) ) ;
#2134 = CARTESIAN_POINT ( 'NONE',  ( 195.0000000000000000, 8.660254037844390851, 140.0000000000000000 ) ) ;
#2135 = CARTESIAN_POINT ( 'NONE',  ( 219.9999999999999716, -25.00000000000000000, 162.5000000000000853 ) ) ;
#2136 = DIRECTION ( 'NONE',  ( -0.000000000000000000, -0.000000000000000000, 1.000000000000000000 ) ) ;
#2137 = DIRECTION ( 'NONE',  ( -0.000000000000000000, -0.000000000000000000, -1.000000000000000000 ) ) ;
#2138 = DIRECTION ( 'NONE',  ( -0.000000000000000000, 1.000000000000000000, -0.000000000000000000 ) ) ;
#2139 = ORIENTED_EDGE ( 'NONE', *, *, #5690, .F. ) ;
#2140 = EDGE_CURVE ( 'NONE', #5732, #2792, #6873, .T. ) ;
#2141 = LINE ( 'NONE', #4434, #730 ) ;
#2142 = DIRECTION ( 'NONE',  ( 0.000000000000000000, 0.000000000000000000, -1.000000000000000000 ) ) ;
#2143 = CARTESIAN_POINT ( 'NONE',  ( 219.9999999999999716, -20.00000000000000000, -162.5000000000000853 ) ) ;
#2144 = DIRECTION ( 'NONE',  ( 0.000000000000000000, 1.224646799147361589E-16, 1.000000000000000000 ) ) ;
#2145 =( LENGTH_UNIT ( ) NAMED_UNIT ( * ) SI_UNIT ( .MILLI., .METRE. ) );
#2146 = CYLINDRICAL_SURFACE ( 'NONE', #5290, 2.649999999999985700 ) ;
#2147 = ORIENTED_EDGE ( 'NONE', *, *, #5344, .F. ) ;
#2148 = ORIENTED_EDGE ( 'NONE', *, *, #2991, .F. ) ;
#2149 = EDGE_CURVE ( 'NONE', #3484, #4485, #5187, .T. ) ;
#2150 = DIRECTION ( 'NONE',  ( 6.123233995736766036E-17, -1.000000000000000000, 0.000000000000000000 ) ) ;
#2151 = ORIENTED_EDGE ( 'NONE', *, *, #5251, .T. ) ;
#2152 =( REPRESENTATION_RELATIONSHIP ('NONE','NONE', #5587, #6025 ) REPRESENTATION_RELATIONSHIP_WITH_TRANSFORMATION ( #5141 )SHAPE_REPRESENTATION_RELATIONSHIP( ) );
#2153 = CARTESIAN_POINT ( 'NONE',  ( 303.3333333333333144, -25.00000000000000000, 165.1500000000000625 ) ) ;
#2154 = EDGE_CURVE ( 'NONE', #3217, #5543, #1085, .T. ) ;
#2155 = CARTESIAN_POINT ( 'NONE',  ( 35.00000000000000000, 8.660254037844390851, 139.9990000000000236 ) ) ;
#2156 = CARTESIAN_POINT ( 'NONE',  ( 136.6666666666666288, -25.00000000000000000, 159.8500000000001080 ) ) ;
#2157 = VERTEX_POINT ( 'NONE', #1319 ) ;
#2158 = AXIS2_PLACEMENT_3D ( 'NONE', #399, #2583, #1040 ) ;
#2159 = PLANE ( 'NONE',  #1478 ) ;
#2160 = DIRECTION ( 'NONE',  ( -0.000000000000000000, 0.000000000000000000, -1.000000000000000000 ) ) ;
#2161 = CARTESIAN_POINT ( 'NONE',  ( 470.0000000000000000, 0.000000000000000000, 145.0000000000000284 ) ) ;
#2162 = DIRECTION ( 'NONE',  ( 1.000000000000000000, 0.000000000000000000, 0.000000000000000000 ) ) ;
#2163 = ORIENTED_EDGE ( 'NONE', *, *, #7005, .T. ) ;
#2164 = EDGE_LOOP ( 'NONE', ( #671, #1560 ) ) ;
#2165 = VERTEX_POINT ( 'NONE', #3558 ) ;
#2166 = DIRECTION ( 'NONE',  ( 1.000000000000000000, 0.000000000000000000, 0.000000000000000000 ) ) ;
#2167 = CARTESIAN_POINT ( 'NONE',  ( -0.02511973781850462134, 4.877415612947412882, -3.751298745799839462 ) ) ;
#2168 = FACE_OUTER_BOUND ( 'NONE', #5066, .T. ) ;
#2169 = DIRECTION ( 'NONE',  ( 1.000000000000000000, 0.000000000000000000, 0.000000000000000000 ) ) ;
#2170 = LINE ( 'NONE', #438, #6628 ) ;
#2171 = UNCERTAINTY_MEASURE_WITH_UNIT (LENGTH_MEASURE( 1.000000000000000082E-05 ), #3079, 'distance_accuracy_value', 'NONE');
#2172 = CARTESIAN_POINT ( 'NONE',  ( 0.000000000000000000, 0.000000000000000000, -4.484454397937119197 ) ) ;
#2173 = AXIS2_PLACEMENT_3D ( 'NONE', #6144, #1608, #3891 ) ;
#2174 = VERTEX_POINT ( 'NONE', #6821 ) ;
#2175 = CARTESIAN_POINT ( 'NONE',  ( -6.259644161404860030E-16, -4.618802153517027165, -3.433295621305388234 ) ) ;
#2176 = CARTESIAN_POINT ( 'NONE',  ( 195.0000000000000000, 8.660254037844390851, 145.0000000000000284 ) ) ;
#2177 = CARTESIAN_POINT ( 'NONE',  ( 1.144235203016666258, 3.958177651039090250, -0.09382832055445661235 ) ) ;
#2178 = DIRECTION ( 'NONE',  ( 0.000000000000000000, 0.000000000000000000, -1.000000000000000000 ) ) ;
#2179 = EDGE_CURVE ( 'NONE', #3697, #2491, #4168, .T. ) ;
#2180 = FACE_OUTER_BOUND ( 'NONE', #3593, .T. ) ;
#2181 = ORIENTED_EDGE ( 'NONE', *, *, #3832, .T. ) ;
#2182 = CIRCLE ( 'NONE', #525, 2.649999999999985700 ) ;
#2183 = ORIENTED_EDGE ( 'NONE', *, *, #3248, .F. ) ;
#2184 = DIRECTION ( 'NONE',  ( 1.000000000000000000, 0.000000000000000000, 0.000000000000000000 ) ) ;
#2185 = VERTEX_POINT ( 'NONE', #5859 ) ;
#2186 = LINE ( 'NONE', #3842, #1034 ) ;
#2187 = AXIS2_PLACEMENT_3D ( 'NONE', #3921, #4525, #35 ) ;
#2188 = CONICAL_SURFACE ( 'NONE', #3494, 4.000000000000000000, 0.8911886515913786111 ) ;
#2189 = AXIS2_PLACEMENT_3D ( 'NONE', #6987, #4093, #2950 ) ;
#2190 = EDGE_CURVE ( 'NONE', #2488, #977, #5788, .T. ) ;
#2191 = LINE ( 'NONE', #2667, #5220 ) ;
#2192 = ADVANCED_FACE ( 'NONE', ( #7026 ), #2755, .F. ) ;
#2193 = EDGE_LOOP ( 'NONE', ( #2510, #5963, #5235, #192 ) ) ;
#2194 = VECTOR ( 'NONE', #1136, 1000.000000000000000 ) ;
#2195 = CARTESIAN_POINT ( 'NONE',  ( 386.6666666666666288, -20.00000000000000000, 162.5000000000000853 ) ) ;
#2196 = CARTESIAN_POINT ( 'NONE',  ( 386.6666666666666288, -25.00000000000000000, -165.1500000000000625 ) ) ;
#2197 = LINE ( 'NONE', #2723, #5096 ) ;
#2198 = DIRECTION ( 'NONE',  ( 1.000000000000000000, 0.000000000000000000, 0.000000000000000000 ) ) ;
#2199 = EDGE_CURVE ( 'NONE', #4599, #3059, #3486, .T. ) ;
#2200 = ORIENTED_EDGE ( 'NONE', *, *, #361, .T. ) ;
#2201 = AXIS2_PLACEMENT_3D ( 'NONE', #2040, #822, #6674 ) ;
#2202 = LINE ( 'NONE', #4501, #1138 ) ;
#2203 = AXIS2_PLACEMENT_3D ( 'NONE', #5418, #3109, #1536 ) ;
#2204 = ORIENTED_EDGE ( 'NONE', *, *, #1049, .T. ) ;
#2205 = VERTEX_POINT ( 'NONE', #5055 ) ;
#2206 = LINE ( 'NONE', #7310, #2963 ) ;
#2207 = CARTESIAN_POINT ( 'NONE',  ( 0.5449313310647804220, 4.304185902836899835, -3.316620875263383894 ) ) ;
#2208 = VECTOR ( 'NONE', #5866, 1000.000000000000000 ) ;
#2209 = ITEM_DEFINED_TRANSFORMATION ( 'NONE', 'NONE', #6813,  #1963 ) ;
#2210 = DIRECTION ( 'NONE',  ( -1.000000000000000000, 0.000000000000000000, 0.000000000000000000 ) ) ;
#2211 = FACE_OUTER_BOUND ( 'NONE', #6930, .T. ) ;
#2212 = CARTESIAN_POINT ( 'NONE',  ( 0.000000000000000000, 0.000000000000000000, 140.0000000000000000 ) ) ;
#2213 = CARTESIAN_POINT ( 'NONE',  ( 0.000000000000000000, 0.000000000000000000, 125.0000000000000000 ) ) ;
#2214 = TOROIDAL_SURFACE ( 'NONE', #6778, 13.29999999999999893, 0.2000000000000027034 ) ;
#2215 = ORIENTED_EDGE ( 'NONE', *, *, #2149, .F. ) ;
#2216 = AXIS2_PLACEMENT_3D ( 'NONE', #6208, #6238, #5117 ) ;
#2217 = CARTESIAN_POINT ( 'NONE',  ( -4.000000000000000000, -2.309401076758512694, -3.433295621305382461 ) ) ;
#2218 = LINE ( 'NONE', #6691, #442 ) ;
#2219 = DIRECTION ( 'NONE',  ( 0.000000000000000000, -0.5000000000000011102, -0.8660254037844379305 ) ) ;
#2220 = DIRECTION ( 'NONE',  ( -0.000000000000000000, 1.000000000000000000, -0.000000000000000000 ) ) ;
#2221 = VECTOR ( 'NONE', #2375, 1000.000000000000114 ) ;
#2222 =( NAMED_UNIT ( * ) SI_UNIT ( $, .STERADIAN. ) SOLID_ANGLE_UNIT ( ) );
#2223 = ORIENTED_EDGE ( 'NONE', *, *, #5444, .T. ) ;
#2224 = ORIENTED_EDGE ( 'NONE', *, *, #4880, .F. ) ;
#2225 = EDGE_CURVE ( 'NONE', #2205, #3050, #666, .T. ) ;
#2227 = VECTOR ( 'NONE', #7179, 1000.000000000000000 ) ;
#2226 = DIRECTION ( 'NONE',  ( 1.000000000000000000, 0.000000000000000000, 0.000000000000000000 ) ) ;
#2228 = ORIENTED_EDGE ( 'NONE', *, *, #819, .F. ) ;
#2229 = DIRECTION ( 'NONE',  ( 1.000000000000000000, 0.000000000000000000, 0.000000000000000000 ) ) ;
#2230 = B_SPLINE_CURVE_WITH_KNOTS ( 'NONE', 3,
 ( #5645, #4528, #2231, #1672, #6250, #3388, #5689, #2989 ),
 .UNSPECIFIED., .F., .F.,
 ( 4, 2, 2, 4 ),
 ( 0.000000000000000000, 0.002450665683189819262, 0.003675998524784728893, 0.004901331366379639391 ),
 .UNSPECIFIED. ) ;
#2231 = CARTESIAN_POINT ( 'NONE',  ( 2.805705207896068476, -3.226868319750173075, -3.503898532754370354 ) ) ;
#2232 = ORIENTED_EDGE ( 'NONE', *, *, #1293, .F. ) ;
#2233 = CARTESIAN_POINT ( 'NONE',  ( 325.0000000000000000, 8.660254037844390851, 139.9990000000000236 ) ) ;
#2234 = EDGE_CURVE ( 'NONE', #4657, #3206, #7099, .T. ) ;
#2235 = CARTESIAN_POINT ( 'NONE',  ( 4.211405965630455661, 2.460463115436283932, -3.751298928144577882 ) ) ;
#2236 = DIRECTION ( 'NONE',  ( 1.000000000000000000, 0.000000000000000000, 0.000000000000000000 ) ) ;
#2237 = ADVANCED_FACE ( 'NONE', ( #6218 ), #2436, .F. ) ;
#2238 = CARTESIAN_POINT ( 'NONE',  ( 136.6666666666666288, -10.00000000000000178, -162.5000000000000853 ) ) ;
#2239 = ORIENTED_EDGE ( 'NONE', *, *, #1650, .F. ) ;
#2240 = DIRECTION ( 'NONE',  ( -1.000000000000000000, 0.000000000000000000, 0.000000000000000000 ) ) ;
#2241 = ORIENTED_EDGE ( 'NONE', *, *, #4287, .F. ) ;
#2242 = ADVANCED_FACE ( 'NONE', ( #3596 ), #4135, .F. ) ;
#2243 = FACE_OUTER_BOUND ( 'NONE', #5727, .T. ) ;
#2244 = CARTESIAN_POINT ( 'NONE',  ( 8.673617379884035472E-16, 4.618802153517012954, -5.000000000000000000 ) ) ;
#2245 = LINE ( 'NONE', #3978, #3480 ) ;
#2246 = DIRECTION ( 'NONE',  ( 0.000000000000000000, 0.000000000000000000, 1.000000000000000000 ) ) ;
#2247 = VERTEX_POINT ( 'NONE', #3350 ) ;
#2248 = DIRECTION ( 'NONE',  ( 0.000000000000000000, 0.000000000000000000, 1.000000000000000000 ) ) ;
#2249 = VERTEX_POINT ( 'NONE', #106 ) ;
#2250 = CYLINDRICAL_SURFACE ( 'NONE', #4673, 11.00000000000000000 ) ;
#2251 = CARTESIAN_POINT ( 'NONE',  ( 386.6666666666666288, -20.00000000000000000, -162.5000000000000853 ) ) ;
#2252 = DIRECTION ( 'NONE',  ( 0.000000000000000000, 0.000000000000000000, -1.000000000000000000 ) ) ;
#2253 = CARTESIAN_POINT ( 'NONE',  ( 1.999999999999998224, 0.000000000000000000, 0.000000000000000000 ) ) ;
#2254 = CARTESIAN_POINT ( 'NONE',  ( -6.259644161404860030E-16, -4.618802153517027165, -5.000000000000000000 ) ) ;
#2255 = ADVANCED_FACE ( 'NONE', ( #2299 ), #2921, .F. ) ;
#2256 = ORIENTED_EDGE ( 'NONE', *, *, #2783, .T. ) ;
#2257 = ORIENTED_EDGE ( 'NONE', *, *, #4935, .T. ) ;
#2258 = APPLICATION_PROTOCOL_DEFINITION ( 'draft international standard', 'automotive_design', 1998, #4252 ) ;
#2259 = VERTEX_POINT ( 'NONE', #6946 ) ;
#2260 = DIRECTION ( 'NONE',  ( -0.000000000000000000, -0.000000000000000000, 1.000000000000000000 ) ) ;
#2261 = ADVANCED_FACE ( 'NONE', ( #4695 ), #1802, .T. ) ;
#2262 = CARTESIAN_POINT ( 'NONE',  ( 0.000000000000000000, 0.000000000000000000, -140.0000000000000000 ) ) ;
#2263 = ORIENTED_EDGE ( 'NONE', *, *, #1115, .T. ) ;
#2264 = CARTESIAN_POINT ( 'NONE',  ( 5.000000000000000888, 0.000000000000000000, 0.000000000000000000 ) ) ;
#2265 = LINE ( 'NONE', #3969, #4014 ) ;
#2266 = VECTOR ( 'NONE', #6681, 1000.000000000000000 ) ;
#2267 = DIRECTION ( 'NONE',  ( 0.000000000000000000, 0.000000000000000000, -1.000000000000000000 ) ) ;
#2268 = EDGE_CURVE ( 'NONE', #7332, #3349, #4477, .T. ) ;
#2269 = ORIENTED_EDGE ( 'NONE', *, *, #4580, .F. ) ;
#2270 = PRODUCT_DEFINITION_SHAPE ( 'NONE', 'NONE',  #7407 ) ;
#2271 = LINE ( 'NONE', #5733, #2896 ) ;
#2272 = EDGE_CURVE ( 'NONE', #1308, #2725, #4840, .T. ) ;
#2273 = VERTEX_POINT ( 'NONE', #7095 ) ;
#2274 = DIRECTION ( 'NONE',  ( 0.000000000000000000, 0.000000000000000000, 1.000000000000000000 ) ) ;
#2275 = CARTESIAN_POINT ( 'NONE',  ( 0.000000000000000000, 0.000000000000000000, -121.0000000000000000 ) ) ;
#2276 = CARTESIAN_POINT ( 'NONE',  ( 5.200000000000002842, 0.000000000000000000, -2.700000000000001066 ) ) ;
#2277 = CARTESIAN_POINT ( 'NONE',  ( 0.000000000000000000, 0.000000000000000000, -140.0000000000000000 ) ) ;
#2278 = CIRCLE ( 'NONE', #33, 13.29999999999999893 ) ;
#2279 = ORIENTED_EDGE ( 'NONE', *, *, #4837, .T. ) ;
#2280 = DIRECTION ( 'NONE',  ( -1.000000000000000000, 0.000000000000000000, 0.000000000000000000 ) ) ;
#2281 = EDGE_CURVE ( 'NONE', #3012, #1563, #1239, .T. ) ;
#2282 = ORIENTED_EDGE ( 'NONE', *, *, #4441, .T. ) ;
#2283 = CARTESIAN_POINT ( 'NONE',  ( 219.9999999999999716, -20.00000000000000000, 162.5000000000000853 ) ) ;
#2284 = FACE_OUTER_BOUND ( 'NONE', #2392, .T. ) ;
#2285 = LINE ( 'NONE', #5180, #1683 ) ;
#2286 = FACE_BOUND ( 'NONE', #6470, .T. ) ;
#2287 = CIRCLE ( 'NONE', #5881, 2.500000000000000444 ) ;
#2288 =( REPRESENTATION_RELATIONSHIP ('NONE','NONE', #5587, #5294 ) REPRESENTATION_RELATIONSHIP_WITH_TRANSFORMATION ( #2098 )SHAPE_REPRESENTATION_RELATIONSHIP( ) );
#2289 = EDGE_CURVE ( 'NONE', #6735, #5434, #5541, .T. ) ;
#2290 = AXIS2_PLACEMENT_3D ( 'NONE', #6120, #2652, #4952 ) ;
#2291 = ORIENTED_EDGE ( 'NONE', *, *, #6513, .F. ) ;
#2292 = CARTESIAN_POINT ( 'NONE',  ( 320.0000000000000000, 0.000000000000000000, -123.0000000000000000 ) ) ;
#2293 = ORIENTED_EDGE ( 'NONE', *, *, #1094, .F. ) ;
#2294 = CARTESIAN_POINT ( 'NONE',  ( 0.000000000000000000, 0.000000000000000000, 0.000000000000000000 ) ) ;
#2295 = DIRECTION ( 'NONE',  ( -0.000000000000000000, -1.000000000000000000, -0.000000000000000000 ) ) ;
#2296 = ORIENTED_EDGE ( 'NONE', *, *, #2956, .F. ) ;
#2297 = FILL_AREA_STYLE ('',( #2957 ) ) ;
#2298 = AXIS2_PLACEMENT_3D ( 'NONE', #2537, #2391, #1870 ) ;
#2299 = FACE_OUTER_BOUND ( 'NONE', #3525, .T. ) ;
#2300 = DIRECTION ( 'NONE',  ( -0.000000000000000000, 1.000000000000000000, 0.000000000000000000 ) ) ;
#2301 = AXIS2_PLACEMENT_3D ( 'NONE', #3746, #7283, #5431 ) ;
#2302 = DIRECTION ( 'NONE',  ( 0.000000000000000000, 0.000000000000000000, 1.000000000000000000 ) ) ;
#2303 = ORIENTED_EDGE ( 'NONE', *, *, #5865, .T. ) ;
#2304 = CARTESIAN_POINT ( 'NONE',  ( -4.211140560182196957, 2.431303136016537803, -3.745885042887433514 ) ) ;
#2305 = CIRCLE ( 'NONE', #656, 2.500000000000000888 ) ;
#2306 = CIRCLE ( 'NONE', #5552, 2.649999999999985700 ) ;
#2307 = EDGE_CURVE ( 'NONE', #468, #1419, #1433, .T. ) ;
#2308 = VERTEX_POINT ( 'NONE', #1471 ) ;
#2309 = DIRECTION ( 'NONE',  ( 1.000000000000000000, 0.000000000000000000, 0.000000000000000000 ) ) ;
#2310 = CARTESIAN_POINT ( 'NONE',  ( 2.500000000000000000, -1.768423874527823569, 1.021000000000002794 ) ) ;
#2311 = ITEM_DEFINED_TRANSFORMATION ( 'NONE', 'NONE', #2409,  #1963 ) ;
#2312 = LINE ( 'NONE', #3470, #268 ) ;
#2313 = DIRECTION ( 'NONE',  ( 0.000000000000000000, -1.000000000000000000, 0.000000000000000000 ) ) ;
#2314 = CIRCLE ( 'NONE', #2539, 2.055000000000000160 ) ;
#2315 =( NAMED_UNIT ( * ) SI_UNIT ( $, .STERADIAN. ) SOLID_ANGLE_UNIT ( ) );
#2316 =( GEOMETRIC_REPRESENTATION_CONTEXT ( 3 ) GLOBAL_UNCERTAINTY_ASSIGNED_CONTEXT ( ( #772 ) ) GLOBAL_UNIT_ASSIGNED_CONTEXT ( ( #4843, #6656, #7134 ) ) REPRESENTATION_CONTEXT ( 'NONE', 'WORKASPACE' ) );
#2317 = EDGE_LOOP ( 'NONE', ( #2854, #4750, #4399, #2393 ) ) ;
#2318 = DIRECTION ( 'NONE',  ( -0.000000000000000000, -1.000000000000000000, -0.000000000000000000 ) ) ;
#2319 = ORIENTED_EDGE ( 'NONE', *, *, #3511, .T. ) ;
#2320 = AXIS2_PLACEMENT_3D ( 'NONE', #1449, #6586, #7269 ) ;
#2321 = CARTESIAN_POINT ( 'NONE',  ( 1.655952806101427033, -3.662737355149048302, -1.182683869819604841E-14 ) ) ;
#2322 = CARTESIAN_POINT ( 'NONE',  ( 0.1404048886732821022, 4.699864953788070565, -3.686887068327037387 ) ) ;
#2323 = LINE ( 'NONE', #6940, #6721 ) ;
#2324 = DIRECTION ( 'NONE',  ( 0.000000000000000000, -0.5000000000000012212, -0.8660254037844380415 ) ) ;
#2325 = ADVANCED_FACE ( 'NONE', ( #3027 ), #7057, .T. ) ;
#2326 = CIRCLE ( 'NONE', #3492, 11.00000000000000000 ) ;
#2327 = LINE ( 'NONE', #4627, #6023 ) ;
#2328 = CIRCLE ( 'NONE', #3030, 2.649999999999985700 ) ;
#2329 = ORIENTED_EDGE ( 'NONE', *, *, #2527, .T. ) ;
#2330 = APPLICATION_PROTOCOL_DEFINITION ( 'draft international standard', 'automotive_design', 1998, #1943 ) ;
#2331 = ORIENTED_EDGE ( 'NONE', *, *, #234, .F. ) ;
#2332 = ADVANCED_FACE ( 'NONE', ( #6011 ), #2543, .T. ) ;
#2333 = VECTOR ( 'NONE', #5204, 1000.000000000000000 ) ;
#2334 = PRODUCT_DEFINITION_SHAPE ( 'NONE', 'NONE',  #7410 ) ;
#2335 = CARTESIAN_POINT ( 'NONE',  ( 395.0000000000000000, -8.660254037844389075, 139.9990000000000236 ) ) ;
#2336 = PRESENTATION_LAYER_ASSIGNMENT (  '', '', ( #6426 ) ) ;
#2337 = ORIENTED_EDGE ( 'NONE', *, *, #440, .T. ) ;
#2338 = DIRECTION ( 'NONE',  ( 0.000000000000000000, 1.000000000000000000, 0.000000000000000000 ) ) ;
#2339 = CARTESIAN_POINT ( 'NONE',  ( 0.000000000000000000, 0.000000000000000000, -125.0000000000000000 ) ) ;
#2340 = ORIENTED_EDGE ( 'NONE', *, *, #1944, .T. ) ;
#2341 = CYLINDRICAL_SURFACE ( 'NONE', #3215, 2.649999999999985700 ) ;
#2342 = EDGE_LOOP ( 'NONE', ( #5280, #338, #5791, #2215 ) ) ;
#2343 = ORIENTED_EDGE ( 'NONE', *, *, #2647, .T. ) ;
#2344 = DIRECTION ( 'NONE',  ( -0.000000000000000000, -0.000000000000000000, 1.000000000000000000 ) ) ;
#2345 = CARTESIAN_POINT ( 'NONE',  ( 219.9999999999999716, -25.00000000000000000, -162.5000000000000853 ) ) ;
#2346 = CARTESIAN_POINT ( 'NONE',  ( 0.000000000000000000, 0.000000000000000000, -5.000000000000000888 ) ) ;
#2347 = DIRECTION ( 'NONE',  ( -0.000000000000000000, -0.000000000000000000, 1.000000000000000000 ) ) ;
#2348 =( NAMED_UNIT ( * ) SI_UNIT ( $, .STERADIAN. ) SOLID_ANGLE_UNIT ( ) );
#2349 = ORIENTED_EDGE ( 'NONE', *, *, #1070, .T. ) ;
#2350 = FACE_OUTER_BOUND ( 'NONE', #3307, .T. ) ;
#2351 = EDGE_CURVE ( 'NONE', #6365, #3602, #7218, .T. ) ;
#2352 = VERTEX_POINT ( 'NONE', #283 ) ;
#2353 = PLANE ( 'NONE',  #5996 ) ;
#2354 = DIRECTION ( 'NONE',  ( -0.000000000000000000, -0.000000000000000000, 1.000000000000000000 ) ) ;
#2355 = CARTESIAN_POINT ( 'NONE',  ( -30.00000000000002842, -20.00000000000000000, 180.0000000000000284 ) ) ;
#2356 = FACE_BOUND ( 'NONE', #1491, .T. ) ;
#2357 = ORIENTED_EDGE ( 'NONE', *, *, #1650, .T. ) ;
#2358 =( LENGTH_UNIT ( ) NAMED_UNIT ( * ) SI_UNIT ( .MILLI., .METRE. ) );
#2359 = EDGE_CURVE ( 'NONE', #918, #5828, #1715, .T. ) ;
#2360 = ORIENTED_EDGE ( 'NONE', *, *, #1406, .T. ) ;
#2361 = CARTESIAN_POINT ( 'NONE',  ( 114.9999999999999858, 8.660254037844390851, 145.0000000000000284 ) ) ;
#2362 = ORIENTED_EDGE ( 'NONE', *, *, #3744, .F. ) ;
#2363 = FILL_AREA_STYLE_COLOUR ( '', #3752 ) ;
#2364 = CARTESIAN_POINT ( 'NONE',  ( -0.6666666666666666297, -4.233901974057276973, -3.300726591567087365 ) ) ;
#2365 = EDGE_CURVE ( 'NONE', #818, #2818, #1948, .T. ) ;
#2366 = ORIENTED_EDGE ( 'NONE', *, *, #5593, .T. ) ;
#2367 = SURFACE_SIDE_STYLE ('',( #4063 ) ) ;
#2368 = EDGE_CURVE ( 'NONE', #7046, #2165, #246, .T. ) ;
#2369 = LINE ( 'NONE', #674, #7245 ) ;
#2370 = LINE ( 'NONE', #1265, #4700 ) ;
#2371 = CYLINDRICAL_SURFACE ( 'NONE', #4140, 12.77499999999999858 ) ;
#2372 = ORIENTED_EDGE ( 'NONE', *, *, #2268, .T. ) ;
#2373 = AXIS2_PLACEMENT_3D ( 'NONE', #2133, #6118, #6000 ) ;
#2374 = DIRECTION ( 'NONE',  ( -0.000000000000000000, 1.000000000000000000, 0.000000000000000000 ) ) ;
#2375 = DIRECTION ( 'NONE',  ( 0.8191520442889902442, 1.003171929053522651E-16, -0.5735764363510482688 ) ) ;
#2376 = CARTESIAN_POINT ( 'NONE',  ( 3.522875095019493141, -2.820352903225631369, -3.598441714920572299 ) ) ;
#2377 = PLANE ( 'NONE',  #2800 ) ;
#2378 =( REPRESENTATION_RELATIONSHIP ('NONE','NONE', #5587, #5294 ) REPRESENTATION_RELATIONSHIP_WITH_TRANSFORMATION ( #2209 )SHAPE_REPRESENTATION_RELATIONSHIP( ) );
#2379 = EDGE_CURVE ( 'NONE', #3960, #5816, #1700, .T. ) ;
#2380 = ORIENTED_EDGE ( 'NONE', *, *, #1222, .T. ) ;
#2381 = DIRECTION ( 'NONE',  ( 0.000000000000000000, 0.000000000000000000, 1.000000000000000000 ) ) ;
#2382 = AXIS2_PLACEMENT_3D ( 'NONE', #5081, #6916, #3416 ) ;
#2383 = VERTEX_POINT ( 'NONE', #6606 ) ;
#2384 = PRODUCT_DEFINITION_SHAPE ( 'NONE', 'NONE',  #7408 ) ;
#2385 = ORIENTED_EDGE ( 'NONE', *, *, #5609, .F. ) ;
#2386 = DIRECTION ( 'NONE',  ( 0.000000000000000000, 1.000000000000000000, -1.471414886128461471E-15 ) ) ;
#2387 = CIRCLE ( 'NONE', #3464, 2.700000000000001066 ) ;
#2388 = CARTESIAN_POINT ( 'NONE',  ( -4.000000000000000000, -0.7890432684750890990, -0.04868663549882315533 ) ) ;
#2389 = DIRECTION ( 'NONE',  ( -0.000000000000000000, 1.471414886128461471E-15, 1.000000000000000000 ) ) ;
#2390 = AXIS2_PLACEMENT_3D ( 'NONE', #5147, #1627, #5630 ) ;
#2391 = DIRECTION ( 'NONE',  ( 1.000000000000000000, 0.000000000000000000, 0.000000000000000000 ) ) ;
#2392 = EDGE_LOOP ( 'NONE', ( #3219, #805, #6638, #11, #6012 ) ) ;
#2393 = ORIENTED_EDGE ( 'NONE', *, *, #319, .F. ) ;
#2394 = DIRECTION ( 'NONE',  ( 0.000000000000000000, 1.000000000000000000, 0.000000000000000000 ) ) ;
#2395 = ORIENTED_EDGE ( 'NONE', *, *, #5314, .F. ) ;
#2396 = EDGE_CURVE ( 'NONE', #7307, #3059, #4878, .T. ) ;
#2397 = CARTESIAN_POINT ( 'NONE',  ( 275.0000000000000000, -8.660254037844389075, 145.0000000000000284 ) ) ;
#2398 = CARTESIAN_POINT ( 'NONE',  ( -6.259644161404860030E-16, -4.618802153517027165, -3.433295621305388234 ) ) ;
#2399 = VERTEX_POINT ( 'NONE', #3637 ) ;
#2400 = DIRECTION ( 'NONE',  ( 1.000000000000000000, 0.000000000000000000, -0.000000000000000000 ) ) ;
#2401 = PRODUCT_DEFINITION_SHAPE ( 'NONE', 'NONE',  #3304 ) ;
#2402 = CARTESIAN_POINT ( 'NONE',  ( 235.0000000000000000, -8.660254037844389075, 145.0000000000000284 ) ) ;
#2403 = EDGE_CURVE ( 'NONE', #1884, #4228, #3792, .T. ) ;
#2404 = TOROIDAL_SURFACE ( 'NONE', #6615, 11.75000000000000000, 1.050000000000000266 ) ;
#2405 = ORIENTED_EDGE ( 'NONE', *, *, #3223, .F. ) ;
#2406 = DIRECTION ( 'NONE',  ( 0.000000000000000000, 0.000000000000000000, -1.000000000000000000 ) ) ;
#2407 = ORIENTED_EDGE ( 'NONE', *, *, #286, .T. ) ;
#2408 = VECTOR ( 'NONE', #4551, 1000.000000000000000 ) ;
#2409 = AXIS2_PLACEMENT_3D ( 'NONE', #1167, #603, #3970 ) ;
#2410 = VECTOR ( 'NONE', #355, 1000.000000000000000 ) ;
#2411 = VECTOR ( 'NONE', #3532, 999.9999999999998863 ) ;
#2412 = CARTESIAN_POINT ( 'NONE',  ( 114.9999999999999858, -8.660254037844389075, 139.9990000000000236 ) ) ;
#2413 = FACE_OUTER_BOUND ( 'NONE', #3179, .T. ) ;
#2414 = FACE_OUTER_BOUND ( 'NONE', #1681, .T. ) ;
#2415 = CARTESIAN_POINT ( 'NONE',  ( 219.9999999999999716, -20.00000000000000000, -162.5000000000000853 ) ) ;
#2416 = EDGE_CURVE ( 'NONE', #1550, #6735, #5364, .T. ) ;
#2417 =( NAMED_UNIT ( * ) PLANE_ANGLE_UNIT ( ) SI_UNIT ( $, .RADIAN. ) );
#2418 = ORIENTED_EDGE ( 'NONE', *, *, #5722, .F. ) ;
#2419 = AXIS2_PLACEMENT_3D ( 'NONE', #2292, #5684, #6920 ) ;
#2420 = CARTESIAN_POINT ( 'NONE',  ( 164.9999999999999716, -8.660254037844389075, 145.0000000000000284 ) ) ;
#2421 = AXIS2_PLACEMENT_3D ( 'NONE', #2155, #4447, #3768 ) ;
#2422 = CIRCLE ( 'NONE', #3244, 2.649999999999985700 ) ;
#2423 = VERTEX_POINT ( 'NONE', #2618 ) ;
#2424 = ORIENTED_EDGE ( 'NONE', *, *, #6184, .F. ) ;
#2425 = DIRECTION ( 'NONE',  ( 0.000000000000000000, -1.000000000000000000, 0.000000000000000000 ) ) ;
#2426 = DIRECTION ( 'NONE',  ( 0.000000000000000000, 0.000000000000000000, 1.000000000000000000 ) ) ;
#2427 = CIRCLE ( 'NONE', #4823, 2.649999999999985700 ) ;
#2428 = PRESENTATION_LAYER_ASSIGNMENT (  '', '', ( #2795 ) ) ;
#2429 = DIRECTION ( 'NONE',  ( 1.000000000000000000, 0.000000000000000000, 0.000000000000000000 ) ) ;
#2430 = DIRECTION ( 'NONE',  ( 0.000000000000000000, -1.000000000000000000, 0.000000000000000000 ) ) ;
#2431 = CARTESIAN_POINT ( 'NONE',  ( 395.0000000000000000, 8.660254037844390851, 139.9990000000000236 ) ) ;
#2432 = AXIS2_PLACEMENT_3D ( 'NONE', #5696, #5729, #6221 ) ;
#2433 = AXIS2_PLACEMENT_3D ( 'NONE', #45, #2302, #6791 ) ;
#2434 = ORIENTED_EDGE ( 'NONE', *, *, #4111, .F. ) ;
#2435 = ITEM_DEFINED_TRANSFORMATION ( 'NONE', 'NONE', #1472,  #1963 ) ;
#2436 = PLANE ( 'NONE',  #59 ) ;
#2437 = ORIENTED_EDGE ( 'NONE', *, *, #1296, .T. ) ;
#2438 = CIRCLE ( 'NONE', #6525, 12.44999999999999929 ) ;
#2439 = CIRCLE ( 'NONE', #2216, 2.649999999999985700 ) ;
#2440 = CARTESIAN_POINT ( 'NONE',  ( -4.000000000000000000, -2.472261339043343220, -3.687027428081192326 ) ) ;
#2441 = ADVANCED_FACE ( 'NONE', ( #4918 ), #2065, .F. ) ;
#2442 = ORIENTED_EDGE ( 'NONE', *, *, #1018, .F. ) ;
#2443 = CIRCLE ( 'NONE', #1631, 13.29999999999999893 ) ;
#2444 = DIRECTION ( 'NONE',  ( -0.000000000000000000, -0.000000000000000000, 1.000000000000000000 ) ) ;
#2445 = VECTOR ( 'NONE', #5726, 1000.000000000000000 ) ;
#2446 = VERTEX_POINT ( 'NONE', #4769 ) ;
#2447 = PRODUCT_DEFINITION_SHAPE ( 'NONE', 'NONE',  #7377 ) ;
#2448 = CARTESIAN_POINT ( 'NONE',  ( 245.0000000000000000, 8.660254037844390851, 145.0000000000000284 ) ) ;
#2449 = ORIENTED_EDGE ( 'NONE', *, *, #2603, .T. ) ;
#2450 = ADVANCED_FACE ( 'NONE', ( #4361 ), #4818, .T. ) ;
#2451 = EDGE_CURVE ( 'NONE', #541, #4054, #6124, .T. ) ;
#2452 = FACE_OUTER_BOUND ( 'NONE', #2762, .T. ) ;
#2453 = AXIS2_PLACEMENT_3D ( 'NONE', #7061, #6329, #7170 ) ;
#2454 = CARTESIAN_POINT ( 'NONE',  ( 470.0000000000000000, -25.00000000000000000, -200.0000000000000000 ) ) ;
#2455 = DIRECTION ( 'NONE',  ( 0.000000000000000000, 0.000000000000000000, 1.000000000000000000 ) ) ;
#2456 = SHAPE_REPRESENTATION_RELATIONSHIP ( 'NONE' , 'NONE' ,  #951, #7090 ) ;
#2457 = ORIENTED_EDGE ( 'NONE', *, *, #4619, .T. ) ;
#2458 = CARTESIAN_POINT ( 'NONE',  ( -4.211140560182196957, -2.431303136016552013, -3.745885042887436178 ) ) ;
#2459 = EDGE_CURVE ( 'NONE', #6041, #3704, #4958, .T. ) ;
#2460 = ORIENTED_EDGE ( 'NONE', *, *, #7052, .T. ) ;
#2461 = ORIENTED_EDGE ( 'NONE', *, *, #395, .T. ) ;
#2462 = CARTESIAN_POINT ( 'NONE',  ( 4.000000000000000000, -2.309401076758514915, -3.433295621305383349 ) ) ;
#2463 = CARTESIAN_POINT ( 'NONE',  ( 0.02511973781850649831, -4.877415612947427981, -3.751298745799844792 ) ) ;
#2464 = CARTESIAN_POINT ( 'NONE',  ( 124.9999999999999858, -8.660254037844389075, 140.0000000000000000 ) ) ;
#2465 = CARTESIAN_POINT ( 'NONE',  ( 219.9999999999999716, -25.00000000000000000, -162.5000000000000853 ) ) ;
#2466 = CARTESIAN_POINT ( 'NONE',  ( 4.000000000000000000, 2.309401076758497151, -3.433295621305379353 ) ) ;
#2467 = CARTESIAN_POINT ( 'NONE',  ( -1.240299975428134203E-15, -4.736529461165891242, -3.681130640444276292 ) ) ;
#2468 = VERTEX_POINT ( 'NONE', #2013 ) ;
#2469 = PRODUCT ( 'roller axis', 'roller axis', '', ( #3485 ) ) ;
#2470 = CONTEXT_DEPENDENT_SHAPE_REPRESENTATION ( #3676, #4875 ) ;
#2471 = DIRECTION ( 'NONE',  ( 0.000000000000000000, 0.000000000000000000, -1.000000000000000000 ) ) ;
#2472 = ORIENTED_EDGE ( 'NONE', *, *, #2628, .F. ) ;
#2473 = EDGE_CURVE ( 'NONE', #5556, #5386, #5468, .T. ) ;
#2474 = DIRECTION ( 'NONE',  ( 0.000000000000000000, 0.000000000000000000, -1.000000000000000000 ) ) ;
#2475 = UNCERTAINTY_MEASURE_WITH_UNIT (LENGTH_MEASURE( 1.000000000000000082E-05 ), #1846, 'distance_accuracy_value', 'NONE');
#2476 = EDGE_LOOP ( 'NONE', ( #969, #6838 ) ) ;
#2477 = ORIENTED_EDGE ( 'NONE', *, *, #3702, .F. ) ;
#2478 = DIRECTION ( 'NONE',  ( -1.000000000000000000, 0.000000000000000000, -0.000000000000000000 ) ) ;
#2479 = DIRECTION ( 'NONE',  ( -0.000000000000000000, 1.000000000000000000, -0.000000000000000000 ) ) ;
#2480 = EDGE_LOOP ( 'NONE', ( #5419, #6968, #5576, #2908 ) ) ;
#2481 = ORIENTED_EDGE ( 'NONE', *, *, #2112, .T. ) ;
#2482 = DIRECTION ( 'NONE',  ( -0.000000000000000000, 1.000000000000000000, -0.000000000000000000 ) ) ;
#2483 = ADVANCED_FACE ( 'NONE', ( #7161 ), #6648, .F. ) ;
#2484 = DIRECTION ( 'NONE',  ( 0.000000000000000000, 0.000000000000000000, -1.000000000000000000 ) ) ;
#2485 = DIRECTION ( 'NONE',  ( -0.000000000000000000, 1.000000000000000000, -0.000000000000000000 ) ) ;
#2486 = DIRECTION ( 'NONE',  ( 1.000000000000000000, 0.000000000000000000, 0.000000000000000000 ) ) ;
#2487 = ADVANCED_FACE ( 'NONE', ( #392 ), #6052, .F. ) ;
#2488 = VERTEX_POINT ( 'NONE', #6687 ) ;
#2489 = DIRECTION ( 'NONE',  ( -0.000000000000000000, -0.000000000000000000, 1.000000000000000000 ) ) ;
#2490 = VECTOR ( 'NONE', #643, 1000.000000000000000 ) ;
#2491 = VERTEX_POINT ( 'NONE', #3127 ) ;
#2492 = VERTEX_POINT ( 'NONE', #3787 ) ;
#2493 = DIRECTION ( 'NONE',  ( -1.000000000000000000, 0.000000000000000000, 0.000000000000000000 ) ) ;
#2494 = CARTESIAN_POINT ( 'NONE',  ( 3.999999999999999112, 1.941961291383486277, -0.3515519931180248192 ) ) ;
#2495 = DIRECTION ( 'NONE',  ( -0.8191520442889875797, 1.003171929053519570E-16, 0.5735764363510522656 ) ) ;
#2496 = DIRECTION ( 'NONE',  ( 1.000000000000000000, 0.000000000000000000, 0.000000000000000000 ) ) ;
#2497 = EDGE_CURVE ( 'NONE', #5368, #1612, #5002, .T. ) ;
#2498 = DIRECTION ( 'NONE',  ( -1.000000000000000000, 0.000000000000000000, 0.000000000000000000 ) ) ;
#2499 = CARTESIAN_POINT ( 'NONE',  ( 53.33333333333330017, -25.00000000000000000, -162.5000000000000853 ) ) ;
#2500 = ORIENTED_EDGE ( 'NONE', *, *, #3370, .T. ) ;
#2501 = VECTOR ( 'NONE', #5149, 1000.000000000000000 ) ;
#2502 = PRESENTATION_LAYER_ASSIGNMENT (  '', '', ( #6472 ) ) ;
#2503 = CONTEXT_DEPENDENT_SHAPE_REPRESENTATION ( #4511, #813 ) ;
#2504 = DIRECTION ( 'NONE',  ( -0.000000000000000000, -0.000000000000000000, 1.000000000000000000 ) ) ;
#2505 = EDGE_LOOP ( 'NONE', ( #6305, #6043 ) ) ;
#2506 =( LENGTH_UNIT ( ) NAMED_UNIT ( * ) SI_UNIT ( .MILLI., .METRE. ) );
#2507 = EDGE_CURVE ( 'NONE', #3965, #4318, #4592, .T. ) ;
#2508 = LINE ( 'NONE', #6097, #5711 ) ;
#2509 = ORIENTED_EDGE ( 'NONE', *, *, #1774, .T. ) ;
#2510 = ORIENTED_EDGE ( 'NONE', *, *, #1284, .T. ) ;
#2511 = CARTESIAN_POINT ( 'NONE',  ( 124.9999999999999858, 8.660254037844390851, 140.0000000000000000 ) ) ;
#2512 = LINE ( 'NONE', #2678, #5198 ) ;
#2513 = AXIS2_PLACEMENT_3D ( 'NONE', #7304, #2160, #6747 ) ;
#2514 = AXIS2_PLACEMENT_3D ( 'NONE', #2264, #4532, #6822 ) ;
#2515 = CARTESIAN_POINT ( 'NONE',  ( 245.0000000000000000, 8.660254037844390851, 140.0000000000000000 ) ) ;
#2516 = LINE ( 'NONE', #4931, #3294 ) ;
#2517 =( REPRESENTATION_RELATIONSHIP ('NONE','NONE', #5587, #5294 ) REPRESENTATION_RELATIONSHIP_WITH_TRANSFORMATION ( #984 )SHAPE_REPRESENTATION_RELATIONSHIP( ) );
#2518 = EDGE_LOOP ( 'NONE', ( #360, #2282 ) ) ;
#2519 = CIRCLE ( 'NONE', #2881, 2.649999999999985700 ) ;
#2520 = LINE ( 'NONE', #2084, #4689 ) ;
#2521 = CARTESIAN_POINT ( 'NONE',  ( 303.3333333333333144, -25.00000000000000000, -162.5000000000000853 ) ) ;
#2522 = DIRECTION ( 'NONE',  ( 0.000000000000000000, 0.000000000000000000, 1.000000000000000000 ) ) ;
#2523 = ORIENTED_EDGE ( 'NONE', *, *, #3458, .T. ) ;
#2524 = CARTESIAN_POINT ( 'NONE',  ( 4.000000000000000000, 2.309401076758497151, -5.000000000000000000 ) ) ;
#2525 = PRODUCT_DEFINITION_SHAPE ( 'NONE', 'NONE',  #7357 ) ;
#2526 = TOROIDAL_SURFACE ( 'NONE', #2994, 10.20000000000000107, 0.2000000000000031197 ) ;
#2527 = EDGE_CURVE ( 'NONE', #1419, #7102, #413, .T. ) ;
#2528 = ORIENTED_EDGE ( 'NONE', *, *, #3035, .F. ) ;
#2529 = ORIENTED_EDGE ( 'NONE', *, *, #2033, .F. ) ;
#2530 = DIRECTION ( 'NONE',  ( 0.000000000000000000, 0.5000000000000012212, 0.8660254037844380415 ) ) ;
#2531 = DIRECTION ( 'NONE',  ( -0.000000000000000000, -1.000000000000000000, -0.000000000000000000 ) ) ;
#2532 = LINE ( 'NONE', #7123, #4205 ) ;
#2533 = DIRECTION ( 'NONE',  ( 0.000000000000000000, 0.000000000000000000, -1.000000000000000000 ) ) ;
#2534 = PRODUCT_DEFINITION_FORMATION_WITH_SPECIFIED_SOURCE ( 'ANY', '', #4155, .NOT_KNOWN. ) ;
#2535 = AXIS2_PLACEMENT_3D ( 'NONE', #4237, #6533, #4913 ) ;
#2536 = AXIS2_PLACEMENT_3D ( 'NONE', #4738, #2794, #178 ) ;
#2537 = CARTESIAN_POINT ( 'NONE',  ( 2.000000000000001776, 0.000000000000000000, 0.000000000000000000 ) ) ;
#2538 = EDGE_LOOP ( 'NONE', ( #6113, #2147 ) ) ;
#2539 = AXIS2_PLACEMENT_3D ( 'NONE', #6598, #5504, #4428 ) ;
#2540 =( GEOMETRIC_REPRESENTATION_CONTEXT ( 3 ) GLOBAL_UNCERTAINTY_ASSIGNED_CONTEXT ( ( #2475 ) ) GLOBAL_UNIT_ASSIGNED_CONTEXT ( ( #1846, #3794, #3711 ) ) REPRESENTATION_CONTEXT ( 'NONE', 'WORKASPACE' ) );
#2541 = ADVANCED_FACE ( 'NONE', ( #6567 ), #7199, .F. ) ;
#2542 = DIRECTION ( 'NONE',  ( -1.000000000000000000, -0.000000000000000000, -0.000000000000000000 ) ) ;
#2543 = CYLINDRICAL_SURFACE ( 'NONE', #3635, 19.00000000000000000 ) ;
#2544 = EDGE_LOOP ( 'NONE', ( #5998, #3659, #458, #5612 ) ) ;
#2545 = CARTESIAN_POINT ( 'NONE',  ( 0.2500000000000002220, 0.000000000000000000, 0.000000000000000000 ) ) ;
#2546 = FILL_AREA_STYLE_COLOUR ( '', #5195 ) ;
#2547 = FACE_OUTER_BOUND ( 'NONE', #6767, .T. ) ;
#2548 = ORIENTED_EDGE ( 'NONE', *, *, #6031, .F. ) ;
#2549 = ADVANCED_FACE ( 'NONE', ( #4430 ), #2737, .F. ) ;
#2550 = VECTOR ( 'NONE', #4413, 1000.000000000000000 ) ;
#2551 = ORIENTED_EDGE ( 'NONE', *, *, #3609, .T. ) ;
#2552 = CARTESIAN_POINT ( 'NONE',  ( 0.000000000000000000, 0.000000000000000000, -4.694516984716113228 ) ) ;
#2553 = DIRECTION ( 'NONE',  ( 0.000000000000000000, -1.000000000000000000, 0.000000000000000000 ) ) ;
#2554 = ADVANCED_FACE ( 'NONE', ( #6601 ), #3495, .T. ) ;
#2555 = CARTESIAN_POINT ( 'NONE',  ( 219.9999999999999716, -20.00000000000000000, -159.8500000000001080 ) ) ;
#2556 = AXIS2_PLACEMENT_3D ( 'NONE', #6850, #5016, #455 ) ;
#2557 = DIRECTION ( 'NONE',  ( -0.000000000000000000, -0.000000000000000000, -1.000000000000000000 ) ) ;
#2558 = AXIS2_PLACEMENT_3D ( 'NONE', #5671, #7287, #2142 ) ;
#2559 = ORIENTED_EDGE ( 'NONE', *, *, #3381, .T. ) ;
#2560 = CARTESIAN_POINT ( 'NONE',  ( 0.000000000000000000, -8.660254037844389075, -140.0000000000000000 ) ) ;
#2561 = CARTESIAN_POINT ( 'NONE',  ( 1.799999999999996048, 0.000000000000000000, 0.000000000000000000 ) ) ;
#2562 = CARTESIAN_POINT ( 'NONE',  ( 355.0000000000000000, 8.660254037844390851, 145.0000000000000284 ) ) ;
#2563 = CIRCLE ( 'NONE', #3526, 10.00000000000000000 ) ;
#2564 = CARTESIAN_POINT ( 'NONE',  ( 303.3333333333333144, -30.00000000000000355, 162.5000000000000853 ) ) ;
#2565 = VERTEX_POINT ( 'NONE', #6724 ) ;
#2566 = CARTESIAN_POINT ( 'NONE',  ( -0.3461262719736137305, 4.658553426539289610, -3.671615880910373608 ) ) ;
#2567 = ORIENTED_EDGE ( 'NONE', *, *, #1306, .F. ) ;
#2568 = VECTOR ( 'NONE', #4068, 1000.000000000000000 ) ;
#2569 = ORIENTED_EDGE ( 'NONE', *, *, #1875, .T. ) ;
#2570 = ORIENTED_EDGE ( 'NONE', *, *, #3757, .T. ) ;
#2571 = DIRECTION ( 'NONE',  ( 1.000000000000000000, 0.000000000000000000, 0.000000000000000000 ) ) ;
#2572 = CARTESIAN_POINT ( 'NONE',  ( 114.9999999999999858, 8.660254037844390851, 139.9990000000000236 ) ) ;
#2573 = CARTESIAN_POINT ( 'NONE',  ( -30.00000000000002842, -15.00000000000000000, 180.0000000000000284 ) ) ;
#2574 = DIRECTION ( 'NONE',  ( -0.000000000000000000, 1.000000000000000000, -0.000000000000000000 ) ) ;
#2575 = EDGE_CURVE ( 'NONE', #5128, #3661, #3001, .T. ) ;
#2576 = CARTESIAN_POINT ( 'NONE',  ( 136.6666666666666288, -20.00000000000000000, 162.5000000000000853 ) ) ;
#2577 = LINE ( 'NONE', #5971, #6637 ) ;
#2578 = AXIS2_PLACEMENT_3D ( 'NONE', #285, #600, #6997 ) ;
#2579 = ORIENTED_EDGE ( 'NONE', *, *, #6613, .F. ) ;
#2580 = LINE ( 'NONE', #2060, #1796 ) ;
#2581 = DIRECTION ( 'NONE',  ( 0.000000000000000000, -1.000000000000000000, 0.000000000000000000 ) ) ;
#2582 = ORIENTED_EDGE ( 'NONE', *, *, #5293, .T. ) ;
#2583 = DIRECTION ( 'NONE',  ( -0.000000000000000000, 0.000000000000000000, -1.000000000000000000 ) ) ;
#2584 = ADVANCED_FACE ( 'NONE', ( #1033 ), #3246, .F. ) ;
#2585 = CARTESIAN_POINT ( 'NONE',  ( 53.33333333333330017, -25.00000000000000000, 165.1500000000000625 ) ) ;
#2586 = EDGE_CURVE ( 'NONE', #5826, #3826, #990, .T. ) ;
#2587 = CARTESIAN_POINT ( 'NONE',  ( 35.00000000000000000, -8.660254037844389075, 140.0000000000000000 ) ) ;
#2588 = ORIENTED_EDGE ( 'NONE', *, *, #701, .T. ) ;
#2589 = DIRECTION ( 'NONE',  ( 1.000000000000000000, 0.000000000000000000, 0.000000000000000000 ) ) ;
#2590 = ORIENTED_EDGE ( 'NONE', *, *, #1840, .F. ) ;
#2591 = PRODUCT_DEFINITION_SHAPE ( 'NONE', 'NONE',  #7364 ) ;
#2592 = DIRECTION ( 'NONE',  ( 0.000000000000000000, -1.000000000000000000, 0.000000000000000000 ) ) ;
#2593 = EDGE_CURVE ( 'NONE', #2887, #6814, #477, .T. ) ;
#2594 = DIRECTION ( 'NONE',  ( 1.000000000000000000, 0.000000000000000000, 0.000000000000000000 ) ) ;
#2595 = CARTESIAN_POINT ( 'NONE',  ( 0.000000000000000000, 0.000000000000000000, 3.469446951953614189E-15 ) ) ;
#2596 = ORIENTED_EDGE ( 'NONE', *, *, #2396, .F. ) ;
#2597 = ADVANCED_FACE ( 'NONE', ( #57 ), #3010, .T. ) ;
#2598 = DIRECTION ( 'NONE',  ( -1.000000000000000000, 0.000000000000000000, 0.000000000000000000 ) ) ;
#2599 = CONTEXT_DEPENDENT_SHAPE_REPRESENTATION ( #349, #4189 ) ;
#2600 = CARTESIAN_POINT ( 'NONE',  ( 386.6666666666666288, -20.00000000000000000, -162.5000000000000853 ) ) ;
#2601 = DIRECTION ( 'NONE',  ( 1.000000000000000000, 0.000000000000000000, 0.000000000000000000 ) ) ;
#2602 = DIRECTION ( 'NONE',  ( -1.000000000000000000, 0.000000000000000000, 0.000000000000000000 ) ) ;
#2603 = EDGE_CURVE ( 'NONE', #6334, #7307, #4513, .T. ) ;
#2604 = ORIENTED_EDGE ( 'NONE', *, *, #7280, .T. ) ;
#2605 = FACE_BOUND ( 'NONE', #6924, .T. ) ;
#2606 = ORIENTED_EDGE ( 'NONE', *, *, #3748, .F. ) ;
#2607 = ORIENTED_EDGE ( 'NONE', *, *, #5953, .T. ) ;
#2608 = DIRECTION ( 'NONE',  ( 0.000000000000000000, 0.4999999999999993339, -0.8660254037844390407 ) ) ;
#2609 = FACE_OUTER_BOUND ( 'NONE', #6661, .T. ) ;
#2610 = DIRECTION ( 'NONE',  ( 0.8191520442889875797, 0.000000000000000000, 0.5735764363510522656 ) ) ;
#2611 = DIRECTION ( 'NONE',  ( -0.000000000000000000, -0.000000000000000000, 1.000000000000000000 ) ) ;
#2612 = ADVANCED_FACE ( 'NONE', ( #4579 ), #5741, .F. ) ;
#2613 = CARTESIAN_POINT ( 'NONE',  ( -20.63749999999999929, 0.000000000000000000, -10.72500000000000142 ) ) ;
#2614 = CARTESIAN_POINT ( 'NONE',  ( 386.6666666666666288, -20.00000000000000000, -165.1500000000000625 ) ) ;
#2615 = DIRECTION ( 'NONE',  ( -0.000000000000000000, 1.000000000000000000, -0.000000000000000000 ) ) ;
#2616 = ORIENTED_EDGE ( 'NONE', *, *, #1189, .F. ) ;
#2617 = DIRECTION ( 'NONE',  ( -1.000000000000000000, 0.000000000000000000, 0.000000000000000000 ) ) ;
#2618 = CARTESIAN_POINT ( 'NONE',  ( 2.500000000000000000, 1.768423874527822681, -1.021000000000002794 ) ) ;
#2619 = EDGE_LOOP ( 'NONE', ( #6575, #4826, #7096, #4865 ) ) ;
#2620 = CARTESIAN_POINT ( 'NONE',  ( -30.00000000000002842, -25.00000000000000000, 200.0000000000000000 ) ) ;
#2621 = VECTOR ( 'NONE', #3085, 1000.000000000000000 ) ;
#2622 = SHAPE_REPRESENTATION_RELATIONSHIP ( 'NONE' , 'NONE' ,  #6025, #402 ) ;
#2623 = CARTESIAN_POINT ( 'NONE',  ( 4.000000000000000000, 2.309401076758515803, -0.4999999999999995559 ) ) ;
#2624 = CARTESIAN_POINT ( 'NONE',  ( -5.000000000000000888, 8.660254037844390851, 150.0000000000000000 ) ) ;
#2625 = AXIS2_PLACEMENT_3D ( 'NONE', #5116, #4582, #617 ) ;
#2626 = COLOUR_RGB ( '',1.000000000000000000, 0.9490196078431372140, 0.9098039215686274384 ) ;
#2627 = ORIENTED_EDGE ( 'NONE', *, *, #4404, .T. ) ;
#2628 = EDGE_CURVE ( 'NONE', #3068, #2674, #177, .T. ) ;
#2629 = CARTESIAN_POINT ( 'NONE',  ( 360.0000000000000000, 0.000000000000000000, 123.0000000000000000 ) ) ;
#2630 = VERTEX_POINT ( 'NONE', #3981 ) ;
#2631 = LINE ( 'NONE', #7140, #5691 ) ;
#2632 = VECTOR ( 'NONE', #2493, 1000.000000000000000 ) ;
#2633 = CARTESIAN_POINT ( 'NONE',  ( 0.000000000000000000, 0.000000000000000000, 121.0000000000000000 ) ) ;
#2634 = PRESENTATION_STYLE_ASSIGNMENT (( #2079 ) ) ;
#2635 = ORIENTED_EDGE ( 'NONE', *, *, #3800, .T. ) ;
#2636 = EDGE_CURVE ( 'NONE', #5227, #6847, #1208, .T. ) ;
#2637 = VECTOR ( 'NONE', #2766, 1000.000000000000000 ) ;
#2638 = CARTESIAN_POINT ( 'NONE',  ( 4.000000000000000888, 0.8228435280416209752, -3.430609588141487976 ) ) ;
#2639 = PLANE ( 'NONE',  #3719 ) ;
#2640 = LINE ( 'NONE', #4381, #1838 ) ;
#2641 = DIRECTION ( 'NONE',  ( 1.000000000000000000, 0.000000000000000000, 0.000000000000000000 ) ) ;
#2642 = ORIENTED_EDGE ( 'NONE', *, *, #4199, .T. ) ;
#2643 = CARTESIAN_POINT ( 'NONE',  ( 19.00000000000000000, 2.326828918379970970E-15, -125.0000000000000000 ) ) ;
#2644 = VECTOR ( 'NONE', #908, 1000.000000000000000 ) ;
#2645 = ORIENTED_EDGE ( 'NONE', *, *, #24, .F. ) ;
#2646 = EDGE_LOOP ( 'NONE', ( #4134, #1236, #5721, #858 ) ) ;
#2647 = EDGE_CURVE ( 'NONE', #76, #1728, #4384, .T. ) ;
#2648 = LINE ( 'NONE', #1542, #2756 ) ;
#2649 = CARTESIAN_POINT ( 'NONE',  ( 2.742827927723449299, 3.035229711104609596, -3.433252694550591233 ) ) ;
#2650 = ADVANCED_FACE ( 'NONE', ( #3474 ), #5627, .F. ) ;
#2651 = CONTEXT_DEPENDENT_SHAPE_REPRESENTATION ( #1894, #6558 ) ;
#2652 = DIRECTION ( 'NONE',  ( 0.000000000000000000, -1.000000000000000000, 0.000000000000000000 ) ) ;
#2653 = DIRECTION ( 'NONE',  ( 0.000000000000000000, 0.000000000000000000, -1.000000000000000000 ) ) ;
#2654 = AXIS2_PLACEMENT_3D ( 'NONE', #6659, #6774, #327 ) ;
#2655 = CARTESIAN_POINT ( 'NONE',  ( 136.6666666666666288, -20.00000000000000000, -162.5000000000000853 ) ) ;
#2656 = DIRECTION ( 'NONE',  ( 0.000000000000000000, 0.000000000000000000, 1.000000000000000000 ) ) ;
#2657 = PRODUCT_DEFINITION ( 'UNKNOWN', '', #2534, #6593 ) ;
#2658 = ORIENTED_EDGE ( 'NONE', *, *, #1768, .T. ) ;
#2659 = PRODUCT_DEFINITION_SHAPE ( 'NONE', 'NONE',  #7370 ) ;
#2660 = CARTESIAN_POINT ( 'NONE',  ( 3.349226789952652439, 2.685125164760731487, -0.2236248678334773199 ) ) ;
#2661 = VECTOR ( 'NONE', #4131, 1000.000000000000000 ) ;
#2662 = CARTESIAN_POINT ( 'NONE',  ( 136.6666666666666288, -20.00000000000000000, 162.5000000000000853 ) ) ;
#2663 = AXIS2_PLACEMENT_3D ( 'NONE', #6065, #7259, #4885 ) ;
#2664 = B_SPLINE_CURVE_WITH_KNOTS ( 'NONE', 3,
 ( #3373, #4625, #5674, #3478, #5780, #555 ),
 .UNSPECIFIED., .F., .F.,
 ( 4, 2, 4 ),
 ( 4.336808689942017736E-19, 0.0002095117440854729585, 0.0004190234881709454834 ),
 .UNSPECIFIED. ) ;
#2665 = DIRECTION ( 'NONE',  ( 0.000000000000000000, 0.000000000000000000, 1.000000000000000000 ) ) ;
#2666 = LINE ( 'NONE', #2744, #5896 ) ;
#2667 = CARTESIAN_POINT ( 'NONE',  ( 35.00000000000000000, -8.660254037844389075, 140.0000000000000000 ) ) ;
#2668 = FACE_BOUND ( 'NONE', #615, .T. ) ;
#2669 = VECTOR ( 'NONE', #3356, 1000.000000000000000 ) ;
#2670 = AXIS2_PLACEMENT_3D ( 'NONE', #5242, #1238, #688 ) ;
#2671 = VERTEX_POINT ( 'NONE', #4544 ) ;
#2672 = ORIENTED_EDGE ( 'NONE', *, *, #3223, .T. ) ;
#2673 = DIRECTION ( 'NONE',  ( 0.000000000000000000, 0.000000000000000000, 1.000000000000000000 ) ) ;
#2674 = VERTEX_POINT ( 'NONE', #649 ) ;
#2675 =( REPRESENTATION_RELATIONSHIP ('NONE','NONE', #5587, #6025 ) REPRESENTATION_RELATIONSHIP_WITH_TRANSFORMATION ( #51 )SHAPE_REPRESENTATION_RELATIONSHIP( ) );
#2676 = VECTOR ( 'NONE', #986, 1000.000000000000000 ) ;
#2677 = PRESENTATION_LAYER_ASSIGNMENT (  '', '', ( #3392 ) ) ;
#2678 = CARTESIAN_POINT ( 'NONE',  ( 25.00000000000000000, 2.516649172247811061E-16, -2.055000000000000160 ) ) ;
#2679 = EDGE_CURVE ( 'NONE', #5999, #1179, #2306, .T. ) ;
#2680 = CARTESIAN_POINT ( 'NONE',  ( -4.000000000000000000, 2.309401076758498483, -3.433295621305379353 ) ) ;
#2681 = VECTOR ( 'NONE', #1338, 1000.000000000000000 ) ;
#2682 = ORIENTED_EDGE ( 'NONE', *, *, #4703, .T. ) ;
#2683 = LINE ( 'NONE', #5020, #1223 ) ;
#2684 = FACE_OUTER_BOUND ( 'NONE', #1694, .T. ) ;
#2685 = CARTESIAN_POINT ( 'NONE',  ( 0.000000000000000000, 0.000000000000000000, 0.000000000000000000 ) ) ;
#2686 = VECTOR ( 'NONE', #2828, 1000.000000000000000 ) ;
#2687 = DIRECTION ( 'NONE',  ( 0.000000000000000000, 0.000000000000000000, 1.000000000000000000 ) ) ;
#2688 = VECTOR ( 'NONE', #2354, 1000.000000000000000 ) ;
#2689 = ORIENTED_EDGE ( 'NONE', *, *, #3035, .T. ) ;
#2690 = FACE_BOUND ( 'NONE', #4445, .T. ) ;
#2691 = EDGE_CURVE ( 'NONE', #4696, #5339, #4597, .T. ) ;
#2692 = ORIENTED_EDGE ( 'NONE', *, *, #5228, .F. ) ;
#2693 = EDGE_LOOP ( 'NONE', ( #6432, #7023, #1911, #5734 ) ) ;
#2694 = CARTESIAN_POINT ( 'NONE',  ( 4.000000000000000000, 2.309401076758497151, -3.433295621305379353 ) ) ;
#2695 = AXIS2_PLACEMENT_3D ( 'NONE', #1172, #4114, #3438 ) ;
#2696 = DIRECTION ( 'NONE',  ( -0.000000000000000000, 1.000000000000000000, -0.000000000000000000 ) ) ;
#2697 = LINE ( 'NONE', #1581, #4929 ) ;
#2698 = CARTESIAN_POINT ( 'NONE',  ( -4.000000000000000000, 0.1981133338132459731, 2.096406544454392723E-17 ) ) ;
#2699 = CARTESIAN_POINT ( 'NONE',  ( 2.500000000000000000, -1.178949249685213863, 2.042000000000002924 ) ) ;
#2700 = DIRECTION ( 'NONE',  ( 1.000000000000000000, 0.000000000000000000, -0.000000000000000000 ) ) ;
#2701 = EDGE_CURVE ( 'NONE', #767, #4657, #6232, .T. ) ;
#2702 = AXIS2_PLACEMENT_3D ( 'NONE', #2595, #4330, #3806 ) ;
#2703 = ORIENTED_EDGE ( 'NONE', *, *, #3757, .F. ) ;
#2704 = DIRECTION ( 'NONE',  ( -0.000000000000000000, 1.000000000000000000, 0.000000000000000000 ) ) ;
#2705 = CARTESIAN_POINT ( 'NONE',  ( 386.6666666666666288, -20.00000000000000000, 165.1500000000000625 ) ) ;
#2706 = FACE_OUTER_BOUND ( 'NONE', #5833, .T. ) ;
#2707 = CARTESIAN_POINT ( 'NONE',  ( 315.0000000000000568, 8.660254037844390851, 145.0000000000000284 ) ) ;
#2708 = PRESENTATION_STYLE_ASSIGNMENT (( #877 ) ) ;
#2709 = SURFACE_SIDE_STYLE ('',( #3212 ) ) ;
#2710 = ADVANCED_BREP_SHAPE_REPRESENTATION ( '', ( #5676, #1963 ), #6040 ) ;
#2711 = VERTEX_POINT ( 'NONE', #6271 ) ;
#2712 = ORIENTED_EDGE ( 'NONE', *, *, #440, .F. ) ;
#2713 = CARTESIAN_POINT ( 'NONE',  ( 386.6666666666666288, -10.00000000000000000, -162.5000000000000853 ) ) ;
#2714 = ORIENTED_EDGE ( 'NONE', *, *, #6878, .F. ) ;
#2715 = DIRECTION ( 'NONE',  ( 0.000000000000000000, 0.000000000000000000, -1.000000000000000000 ) ) ;
#2716 = ADVANCED_FACE ( 'NONE', ( #1762 ), #6283, .T. ) ;
#2717 = CARTESIAN_POINT ( 'NONE',  ( -4.000000000000004441, 2.309401076758496263, -3.504269196027523847 ) ) ;
#2718 = CARTESIAN_POINT ( 'NONE',  ( 386.6666666666666288, -20.00000000000000000, -162.5000000000000853 ) ) ;
#2719 = ORIENTED_EDGE ( 'NONE', *, *, #5305, .T. ) ;
#2720 = CARTESIAN_POINT ( 'NONE',  ( 5.000000000000004441, 0.000000000000000000, 4.250000000000000000 ) ) ;
#2721 = EDGE_CURVE ( 'NONE', #6469, #6561, #2186, .T. ) ;
#2722 = CARTESIAN_POINT ( 'NONE',  ( 1.734723475976807094E-15, 4.618802153517012954, -0.4999999999999995559 ) ) ;
#2723 = CARTESIAN_POINT ( 'NONE',  ( -5.560781378645573980, 0.000000000000000000, -4.000000000000000000 ) ) ;
#2724 = CARTESIAN_POINT ( 'NONE',  ( 80.00000000000000000, 0.000000000000000000, -123.0000000000000000 ) ) ;
#2725 = VERTEX_POINT ( 'NONE', #22 ) ;
#2726 = CARTESIAN_POINT ( 'NONE',  ( 4.999999999999999112, 8.660254037844390851, 139.9990000000000236 ) ) ;
#2727 = ORIENTED_EDGE ( 'NONE', *, *, #7004, .T. ) ;
#2728 = EDGE_CURVE ( 'NONE', #6875, #3397, #538, .T. ) ;
#2729 = ORIENTED_EDGE ( 'NONE', *, *, #4854, .T. ) ;
#2730 = CARTESIAN_POINT ( 'NONE',  ( 4.203833317240879275, 1.627343821129582979, -3.597273115243889929 ) ) ;
#2731 = DIRECTION ( 'NONE',  ( -0.000000000000000000, -0.000000000000000000, 1.000000000000000000 ) ) ;
#2732 = ITEM_DEFINED_TRANSFORMATION ( 'NONE', 'NONE', #5073,  #1963 ) ;
#2733 = DIRECTION ( 'NONE',  ( -1.000000000000000000, -0.000000000000000000, -0.000000000000000000 ) ) ;
#2734 = DIRECTION ( 'NONE',  ( 0.000000000000000000, 0.000000000000000000, -1.000000000000000000 ) ) ;
#2735 = EDGE_CURVE ( 'NONE', #4758, #4011, #509, .T. ) ;
#2736 = FACE_OUTER_BOUND ( 'NONE', #5972, .T. ) ;
#2737 = PLANE ( 'NONE',  #6273 ) ;
#2738 = ORIENTED_EDGE ( 'NONE', *, *, #5305, .F. ) ;
#2739 = CARTESIAN_POINT ( 'NONE',  ( 0.000000000000000000, 0.000000000000000000, 140.0000000000000000 ) ) ;
#2740 = CARTESIAN_POINT ( 'NONE',  ( 219.9999999999999716, -14.99999999999999822, 165.1500000000000625 ) ) ;
#2741 = CARTESIAN_POINT ( 'NONE',  ( -0.3198814748697807464, -4.434118497892185040, -0.3507732604232532969 ) ) ;
#2742 = LINE ( 'NONE', #876, #4439 ) ;
#2743 = ADVANCED_FACE ( 'NONE', ( #5710 ), #1069, .T. ) ;
#2744 = CARTESIAN_POINT ( 'NONE',  ( 5.560781378645573980, 6.809993116116507654E-16, -4.000000000000000000 ) ) ;
#2745 = ORIENTED_EDGE ( 'NONE', *, *, #1613, .T. ) ;
#2746 = ORIENTED_EDGE ( 'NONE', *, *, #6777, .T. ) ;
#2747 = TOROIDAL_SURFACE ( 'NONE', #7059, 13.29999999999999893, 0.2000000000000027034 ) ;
#2748 = DIRECTION ( 'NONE',  ( 0.000000000000000000, 0.000000000000000000, 1.000000000000000000 ) ) ;
#2749 = VERTEX_POINT ( 'NONE', #2842 ) ;
#2750 = ADVANCED_FACE ( 'NONE', ( #1101 ), #1825, .F. ) ;
#2751 = DIRECTION ( 'NONE',  ( -1.000000000000000000, -0.000000000000000000, -0.000000000000000000 ) ) ;
#2752 = CIRCLE ( 'NONE', #1569, 2.649999999999985700 ) ;
#2753 = DIRECTION ( 'NONE',  ( -0.000000000000000000, -0.000000000000000000, 1.000000000000000000 ) ) ;
#2754 = ORIENTED_EDGE ( 'NONE', *, *, #6883, .F. ) ;
#2755 = PLANE ( 'NONE',  #1734 ) ;
#2756 = VECTOR ( 'NONE', #4425, 1000.000000000000000 ) ;
#2757 = DIRECTION ( 'NONE',  ( -1.000000000000000000, 0.000000000000000000, 0.000000000000000000 ) ) ;
#2758 = CARTESIAN_POINT ( 'NONE',  ( 136.6666666666666288, -20.00000000000000000, -159.8500000000001080 ) ) ;
#2759 = CARTESIAN_POINT ( 'NONE',  ( 200.0000000000000000, 0.000000000000000000, 123.0000000000000000 ) ) ;
#2760 = ORIENTED_EDGE ( 'NONE', *, *, #4565, .F. ) ;
#2761 = CARTESIAN_POINT ( 'NONE',  ( 0.000000000000000000, 0.000000000000000000, -140.0000000000000000 ) ) ;
#2762 = EDGE_LOOP ( 'NONE', ( #6483, #2340, #5301, #2094 ) ) ;
#2763 = EDGE_LOOP ( 'NONE', ( #3110, #4745 ) ) ;
#2764 = DIRECTION ( 'NONE',  ( -1.000000000000000000, -0.000000000000000000, -0.000000000000000000 ) ) ;
#2765 = DIRECTION ( 'NONE',  ( -1.000000000000000000, 0.000000000000000000, 0.000000000000000000 ) ) ;
#2766 = DIRECTION ( 'NONE',  ( -1.000000000000000000, 0.000000000000000000, 0.000000000000000000 ) ) ;
#2767 = LINE ( 'NONE', #19, #2194 ) ;
#2768 = DIRECTION ( 'NONE',  ( -1.000000000000000000, -0.000000000000000000, -0.000000000000000000 ) ) ;
#2769 = DIRECTION ( 'NONE',  ( -1.000000000000000000, -0.000000000000000000, -0.000000000000000000 ) ) ;
#2770 = ADVANCED_FACE ( 'NONE', ( #7078 ), #5912, .F. ) ;
#2771 = AXIS2_PLACEMENT_3D ( 'NONE', #148, #6538, #2855 ) ;
#2772 =( REPRESENTATION_RELATIONSHIP ('NONE','NONE', #5587, #5023 ) REPRESENTATION_RELATIONSHIP_WITH_TRANSFORMATION ( #3026 )SHAPE_REPRESENTATION_RELATIONSHIP( ) );
#2773 = VERTEX_POINT ( 'NONE', #6969 ) ;
#2774 = DIRECTION ( 'NONE',  ( 0.000000000000000000, 0.000000000000000000, 1.000000000000000000 ) ) ;
#2775 = DIRECTION ( 'NONE',  ( 0.000000000000000000, 0.000000000000000000, 1.000000000000000000 ) ) ;
#2776 = CARTESIAN_POINT ( 'NONE',  ( -2.000000000000007550, -3.464101615137749945, 0.000000000000000000 ) ) ;
#2777 = FACE_BOUND ( 'NONE', #963, .T. ) ;
#2778 = AXIS2_PLACEMENT_3D ( 'NONE', #6284, #5783, #6349 ) ;
#2779 = EDGE_CURVE ( 'NONE', #3365, #2803, #748, .T. ) ;
#2780 = ORIENTED_EDGE ( 'NONE', *, *, #6537, .F. ) ;
#2781 = AXIS2_PLACEMENT_3D ( 'NONE', #1837, #5823, #1314 ) ;
#2782 = ORIENTED_EDGE ( 'NONE', *, *, #4396, .F. ) ;
#2783 = EDGE_CURVE ( 'NONE', #1288, #431, #1358, .T. ) ;
#2784 = ORIENTED_EDGE ( 'NONE', *, *, #337, .F. ) ;
#2785 = CARTESIAN_POINT ( 'NONE',  ( 1.999999999999997335, 10.20000000000000107, 0.000000000000000000 ) ) ;
#2786 = VECTOR ( 'NONE', #3616, 1000.000000000000000 ) ;
#2787 = LINE ( 'NONE', #5051, #7118 ) ;
#2788 = CIRCLE ( 'NONE', #5304, 2.649999999999985700 ) ;
#2789 = VECTOR ( 'NONE', #4641, 1000.000000000000000 ) ;
#2790 = DIRECTION ( 'NONE',  ( 0.000000000000000000, -1.000000000000000000, 0.000000000000000000 ) ) ;
#2791 = EDGE_CURVE ( 'NONE', #6671, #7155, #1341, .T. ) ;
#2792 = VERTEX_POINT ( 'NONE', #233 ) ;
#2793 = AXIS2_PLACEMENT_3D ( 'NONE', #831, #3088, #3518 ) ;
#2794 = DIRECTION ( 'NONE',  ( -1.000000000000000000, -0.000000000000000000, -0.000000000000000000 ) ) ;
#2795 = STYLED_ITEM ( 'NONE', ( #7327 ), #5044 ) ;
#2796 = LINE ( 'NONE', #2827, #4704 ) ;
#2797 = CARTESIAN_POINT ( 'NONE',  ( 386.6666666666666288, -14.99999999999999822, 162.5000000000000853 ) ) ;
#2798 = CARTESIAN_POINT ( 'NONE',  ( 53.33333333333330017, -10.00000000000000000, -162.5000000000000853 ) ) ;
#2799 = ORIENTED_EDGE ( 'NONE', *, *, #3881, .F. ) ;
#2800 = AXIS2_PLACEMENT_3D ( 'NONE', #3618, #4151, #4182 ) ;
#2801 = CARTESIAN_POINT ( 'NONE',  ( 155.0000000000000000, 8.660254037844390851, 140.0000000000000000 ) ) ;
#2802 = AXIS2_PLACEMENT_3D ( 'NONE', #3354, #4605, #5652 ) ;
#2803 = VERTEX_POINT ( 'NONE', #5815 ) ;
#2804 = DIRECTION ( 'NONE',  ( -1.000000000000000000, 0.000000000000000000, 0.000000000000000000 ) ) ;
#2805 = FACE_OUTER_BOUND ( 'NONE', #4089, .T. ) ;
#2806 = CONICAL_SURFACE ( 'NONE', #75, 4.000000000000000000, 0.8911886515913786111 ) ;
#2807 = DIRECTION ( 'NONE',  ( 0.000000000000000000, 1.000000000000000000, 0.000000000000000000 ) ) ;
#2808 = DIRECTION ( 'NONE',  ( 1.000000000000000000, 0.000000000000000000, 0.000000000000000000 ) ) ;
#2809 = CIRCLE ( 'NONE', #5811, 4.000000000000000000 ) ;
#2810 = EDGE_LOOP ( 'NONE', ( #5349, #6944, #1467 ) ) ;
#2811 = DIRECTION ( 'NONE',  ( 0.000000000000000000, 0.000000000000000000, -1.000000000000000000 ) ) ;
#2812 = ORIENTED_EDGE ( 'NONE', *, *, #260, .F. ) ;
#2813 = CARTESIAN_POINT ( 'NONE',  ( 235.0000000000000000, 8.660254037844390851, 145.0000000000000284 ) ) ;
#2814 = DIRECTION ( 'NONE',  ( 0.000000000000000000, 0.000000000000000000, 1.000000000000000000 ) ) ;
#2815 = EDGE_CURVE ( 'NONE', #6064, #2249, #1891, .T. ) ;
#2816 = FACE_OUTER_BOUND ( 'NONE', #1446, .T. ) ;
#2817 = DIRECTION ( 'NONE',  ( -1.000000000000000000, -0.000000000000000000, -0.000000000000000000 ) ) ;
#2818 = VERTEX_POINT ( 'NONE', #2420 ) ;
#2819 = ORIENTED_EDGE ( 'NONE', *, *, #638, .T. ) ;
#2820 = AXIS2_PLACEMENT_3D ( 'NONE', #1605, #3925, #5574 ) ;
#2821 = VERTEX_POINT ( 'NONE', #5925 ) ;
#2822 = EDGE_CURVE ( 'NONE', #7233, #1000, #3749, .T. ) ;
#2823 = LINE ( 'NONE', #1599, #2550 ) ;
#2824 = EDGE_CURVE ( 'NONE', #4123, #4841, #2422, .T. ) ;
#2825 = CARTESIAN_POINT ( 'NONE',  ( 435.0000000000000568, -8.660254037844389075, 140.0000000000000000 ) ) ;
#2826 = VERTEX_POINT ( 'NONE', #4680 ) ;
#2827 = CARTESIAN_POINT ( 'NONE',  ( 355.0000000000000000, 8.660254037844390851, 140.0000000000000000 ) ) ;
#2828 = DIRECTION ( 'NONE',  ( -1.000000000000000000, -0.000000000000000000, -0.000000000000000000 ) ) ;
#2829 = ADVANCED_FACE ( 'NONE', ( #5319, #1277 ), #6523, .F. ) ;
#2830 = CARTESIAN_POINT ( 'NONE',  ( 120.0000000000000000, 0.000000000000000000, 123.0000000000000000 ) ) ;
#2831 = ORIENTED_EDGE ( 'NONE', *, *, #2179, .T. ) ;
#2832 = CARTESIAN_POINT ( 'NONE',  ( -5.000000000000000888, 8.660254037844390851, 140.0000000000000000 ) ) ;
#2833 = AXIS2_PLACEMENT_3D ( 'NONE', #3117, #4761, #5388 ) ;
#2834 = ORIENTED_EDGE ( 'NONE', *, *, #7031, .F. ) ;
#2835 = CARTESIAN_POINT ( 'NONE',  ( 0.000000000000000000, 0.000000000000000000, 125.0000000000000000 ) ) ;
#2836 = PLANE ( 'NONE',  #789 ) ;
#2837 = CONTEXT_DEPENDENT_SHAPE_REPRESENTATION ( #3041, #1909 ) ;
#2838 = DIRECTION ( 'NONE',  ( 0.000000000000000000, 0.000000000000000000, 1.000000000000000000 ) ) ;
#2839 = CARTESIAN_POINT ( 'NONE',  ( 0.2500000000000002220, 4.898587196589412829E-16, -4.000000000000000000 ) ) ;
#2840 = EDGE_CURVE ( 'NONE', #224, #2007, #2182, .T. ) ;
#2841 = EDGE_LOOP ( 'NONE', ( #7003, #5682 ) ) ;
#2842 = CARTESIAN_POINT ( 'NONE',  ( 1.999999999999998668, 0.000000000000000000, -10.20000000000000107 ) ) ;
#2843 = EDGE_LOOP ( 'NONE', ( #886, #2263, #6993, #7228 ) ) ;
#2844 = FACE_BOUND ( 'NONE', #6308, .T. ) ;
#2845 = DIRECTION ( 'NONE',  ( 0.000000000000000000, 0.000000000000000000, 1.000000000000000000 ) ) ;
#2846 = DIRECTION ( 'NONE',  ( 0.000000000000000000, 0.000000000000000000, 1.000000000000000000 ) ) ;
#2847 = DIRECTION ( 'NONE',  ( 0.000000000000000000, 1.000000000000000000, 0.000000000000000000 ) ) ;
#2848 = CARTESIAN_POINT ( 'NONE',  ( 0.000000000000000000, 0.000000000000000000, 140.0000000000000000 ) ) ;
#2849 = ORIENTED_EDGE ( 'NONE', *, *, #2586, .F. ) ;
#2850 = ORIENTED_EDGE ( 'NONE', *, *, #6068, .F. ) ;
#2851 = LINE ( 'NONE', #6248, #5439 ) ;
#2852 = DIRECTION ( 'NONE',  ( 0.000000000000000000, -1.000000000000000000, 0.000000000000000000 ) ) ;
#2853 = ADVANCED_FACE ( 'NONE', ( #4121 ), #716, .F. ) ;
#2854 = ORIENTED_EDGE ( 'NONE', *, *, #1014, .F. ) ;
#2855 = DIRECTION ( 'NONE',  ( 0.000000000000000000, 0.000000000000000000, 1.000000000000000000 ) ) ;
#2856 = CARTESIAN_POINT ( 'NONE',  ( -5.000000000000000888, 8.660254037844390851, -150.0000000000000000 ) ) ;
#2857 = AXIS2_PLACEMENT_3D ( 'NONE', #6864, #5108, #3437 ) ;
#2858 = DIRECTION ( 'NONE',  ( -1.000000000000000000, -6.123233995736766036E-17, -6.123233995736764803E-17 ) ) ;
#2859 = ORIENTED_EDGE ( 'NONE', *, *, #6351, .F. ) ;
#2860 = DIRECTION ( 'NONE',  ( -1.000000000000000000, 0.000000000000000000, 0.000000000000000000 ) ) ;
#2861 = CIRCLE ( 'NONE', #2382, 2.649999999999985700 ) ;
#2862 = ADVANCED_FACE ( 'NONE', ( #2350 ), #2404, .T. ) ;
#2863 = ORIENTED_EDGE ( 'NONE', *, *, #6967, .F. ) ;
#2864 = EDGE_CURVE ( 'NONE', #828, #224, #5279, .T. ) ;
#2865 = CARTESIAN_POINT ( 'NONE',  ( -5.000000000000000888, 8.660254037844387298, -140.0000000000000000 ) ) ;
#2866 = DIRECTION ( 'NONE',  ( -0.000000000000000000, 1.000000000000000000, -0.000000000000000000 ) ) ;
#2867 = ITEM_DEFINED_TRANSFORMATION ( 'NONE', 'NONE', #5902,  #1963 ) ;
#2868 = DIRECTION ( 'NONE',  ( -0.000000000000000000, 1.000000000000000000, -0.000000000000000000 ) ) ;
#2869 = CARTESIAN_POINT ( 'NONE',  ( 303.3333333333333144, -14.99999999999999822, 165.1500000000000625 ) ) ;
#2870 =( NAMED_UNIT ( * ) PLANE_ANGLE_UNIT ( ) SI_UNIT ( $, .RADIAN. ) );
#2871 = ORIENTED_EDGE ( 'NONE', *, *, #6234, .T. ) ;
#2872 = CARTESIAN_POINT ( 'NONE',  ( 1.800000000000001155, 0.000000000000000000, 0.000000000000000000 ) ) ;
#2873 = ADVANCED_FACE ( 'NONE', ( #3577 ), #2526, .T. ) ;
#2874 = VERTEX_POINT ( 'NONE', #793 ) ;
#2875 = FACE_OUTER_BOUND ( 'NONE', #4066, .T. ) ;
#2876 = CARTESIAN_POINT ( 'NONE',  ( 275.0000000000000000, -8.660254037844389075, 139.9990000000000236 ) ) ;
#2877 = CARTESIAN_POINT ( 'NONE',  ( -11.00000000000000000, 0.000000000000000000, -121.0000000000000000 ) ) ;
#2878 = CARTESIAN_POINT ( 'NONE',  ( -1.999999999999998224, 0.000000000000000000, -11.05000000000000071 ) ) ;
#2879 = VECTOR ( 'NONE', #1859, 1000.000000000000000 ) ;
#2880 = CARTESIAN_POINT ( 'NONE',  ( -4.000000000000000888, -1.539600717839011201, -3.300726591567081591 ) ) ;
#2881 = AXIS2_PLACEMENT_3D ( 'NONE', #2135, #4308, #6597 ) ;
#2882 = ORIENTED_EDGE ( 'NONE', *, *, #3341, .T. ) ;
#2883 = DIRECTION ( 'NONE',  ( -1.000000000000000000, 0.000000000000000000, 0.000000000000000000 ) ) ;
#2884 = VERTEX_POINT ( 'NONE', #901 ) ;
#2885 = MECHANICAL_DESIGN_GEOMETRIC_PRESENTATION_REPRESENTATION (  '', ( #6746 ), #6383 ) ;
#2886 = CARTESIAN_POINT ( 'NONE',  ( -3.999999999998910649, -1.658469974638591804, -3.531532913075256186 ) ) ;
#2887 = VERTEX_POINT ( 'NONE', #5536 ) ;
#2888 = AXIS2_PLACEMENT_3D ( 'NONE', #3801, #407, #7174 ) ;
#2889 = EDGE_CURVE ( 'NONE', #4692, #709, #6810, .T. ) ;
#2890 = CARTESIAN_POINT ( 'NONE',  ( 0.000000000000000000, 0.000000000000000000, 3.469446951953614189E-15 ) ) ;
#2891 = AXIS2_PLACEMENT_3D ( 'NONE', #7219, #4375, #1050 ) ;
#2892 = VERTEX_POINT ( 'NONE', #2643 ) ;
#2893 = DIRECTION ( 'NONE',  ( 1.000000000000000000, 0.000000000000000000, 0.000000000000000000 ) ) ;
#2894 = CIRCLE ( 'NONE', #7106, 0.2000000000000022593 ) ;
#2895 = ORIENTED_EDGE ( 'NONE', *, *, #5380, .T. ) ;
#2896 = VECTOR ( 'NONE', #5062, 1000.000000000000000 ) ;
#2897 = EDGE_LOOP ( 'NONE', ( #1648, #6143, #1219 ) ) ;
#2898 = FACE_OUTER_BOUND ( 'NONE', #2034, .T. ) ;
#2899 = CARTESIAN_POINT ( 'NONE',  ( 235.0000000000000000, -8.660254037844389075, 140.0000000000000000 ) ) ;
#2900 = ITEM_DEFINED_TRANSFORMATION ( 'NONE', 'NONE', #2999,  #1963 ) ;
#2901 = DIRECTION ( 'NONE',  ( 0.000000000000000000, -1.000000000000000000, 0.000000000000000000 ) ) ;
#2902 = DIRECTION ( 'NONE',  ( 1.000000000000000000, 0.000000000000000000, 0.000000000000000000 ) ) ;
#2903 =( REPRESENTATION_RELATIONSHIP ('NONE','NONE', #5587, #6025 ) REPRESENTATION_RELATIONSHIP_WITH_TRANSFORMATION ( #6033 )SHAPE_REPRESENTATION_RELATIONSHIP( ) );
#2904 = AXIS2_PLACEMENT_3D ( 'NONE', #3726, #6708, #1573 ) ;
#2905 = SURFACE_STYLE_FILL_AREA ( #400 ) ;
#2906 = MECHANICAL_DESIGN_GEOMETRIC_PRESENTATION_REPRESENTATION (  '', ( #670 ), #4713 ) ;
#2907 = EDGE_CURVE ( 'NONE', #4971, #6875, #3159, .T. ) ;
#2908 = ORIENTED_EDGE ( 'NONE', *, *, #260, .T. ) ;
#2909 = CARTESIAN_POINT ( 'NONE',  ( 0.000000000000000000, 0.000000000000000000, -125.0000000000000000 ) ) ;
#2910 = VERTEX_POINT ( 'NONE', #344 ) ;
#2911 = VECTOR ( 'NONE', #1264, 1000.000000000000000 ) ;
#2912 = FACE_OUTER_BOUND ( 'NONE', #1403, .T. ) ;
#2913 = DIRECTION ( 'NONE',  ( 0.000000000000000000, 0.000000000000000000, 1.000000000000000000 ) ) ;
#2914 = DIRECTION ( 'NONE',  ( -0.000000000000000000, 1.000000000000000000, -0.000000000000000000 ) ) ;
#2915 = ADVANCED_FACE ( 'NONE', ( #3777 ), #7230, .T. ) ;
#2916 = CARTESIAN_POINT ( 'NONE',  ( 395.0000000000000000, -8.660254037844389075, 140.0000000000000000 ) ) ;
#2917 = VECTOR ( 'NONE', #3066, 1000.000000000000000 ) ;
#2918 = EDGE_CURVE ( 'NONE', #1142, #4696, #1595, .T. ) ;
#2919 = EDGE_LOOP ( 'NONE', ( #6079, #6549, #6953, #3320, #2569 ) ) ;
#2920 =( NAMED_UNIT ( * ) PLANE_ANGLE_UNIT ( ) SI_UNIT ( $, .RADIAN. ) );
#2921 = CYLINDRICAL_SURFACE ( 'NONE', #1126, 2.500000000000000444 ) ;
#2922 = ORIENTED_EDGE ( 'NONE', *, *, #54, .F. ) ;
#2923 = PRODUCT_DEFINITION_SHAPE ( 'NONE', 'NONE',  #7409 ) ;
#2924 = DIRECTION ( 'NONE',  ( 0.000000000000000000, 0.000000000000000000, 1.000000000000000000 ) ) ;
#2925 = PLANE ( 'NONE',  #7133 ) ;
#2926 = CIRCLE ( 'NONE', #1160, 2.649999999999985700 ) ;
#2927 = EDGE_LOOP ( 'NONE', ( #1912, #5411, #4848, #6287 ) ) ;
#2928 = ADVANCED_FACE ( 'NONE', ( #1973, #7190 ), #854, .T. ) ;
#2929 = DIRECTION ( 'NONE',  ( 1.000000000000000000, 0.000000000000000000, 0.000000000000000000 ) ) ;
#2930 = LINE ( 'NONE', #2515, #4812 ) ;
#2931 = CARTESIAN_POINT ( 'NONE',  ( 219.9999999999999716, -25.00000000000000000, 159.8500000000001080 ) ) ;
#2932 = ORIENTED_EDGE ( 'NONE', *, *, #5619, .T. ) ;
#2933 = CYLINDRICAL_SURFACE ( 'NONE', #3953, 2.500000000000000444 ) ;
#2934 = DIRECTION ( 'NONE',  ( 0.000000000000000000, -0.000000000000000000, 1.000000000000000000 ) ) ;
#2935 = DIRECTION ( 'NONE',  ( 0.000000000000000000, -1.000000000000000000, 0.000000000000000000 ) ) ;
#2936 = DIRECTION ( 'NONE',  ( 0.000000000000000000, 0.000000000000000000, 1.000000000000000000 ) ) ;
#2937 = SURFACE_STYLE_USAGE ( .BOTH. , #3575 ) ;
#2938 = ORIENTED_EDGE ( 'NONE', *, *, #5000, .F. ) ;
#2939 = CARTESIAN_POINT ( 'NONE',  ( 205.0000000000000284, 8.660254037844390851, 139.9990000000000236 ) ) ;
#2940 = EDGE_CURVE ( 'NONE', #478, #5732, #3488, .T. ) ;
#2941 = ORIENTED_EDGE ( 'NONE', *, *, #1018, .T. ) ;
#2942 = DIRECTION ( 'NONE',  ( -0.000000000000000000, 1.000000000000000000, 0.000000000000000000 ) ) ;
#2943 = CARTESIAN_POINT ( 'NONE',  ( -1.243802165048909503, 3.900692638707381921, -3.223146290109805800 ) ) ;
#2944 = DIRECTION ( 'NONE',  ( 0.000000000000000000, -0.4999999999999993894, 0.8660254037844389297 ) ) ;
#2945 = CARTESIAN_POINT ( 'NONE',  ( 303.3333333333333144, -20.00000000000000000, 162.5000000000000853 ) ) ;
#2946 = PLANE ( 'NONE',  #3989 ) ;
#2947 = B_SPLINE_CURVE_WITH_KNOTS ( 'NONE', 3,
 ( #4009, #499, #3463, #5164, #605, #2304 ),
 .UNSPECIFIED., .F., .F.,
 ( 4, 2, 4 ),
 ( 0.002452478801916376308, 0.003676905084148007850, 0.004901331366379639391 ),
 .UNSPECIFIED. ) ;
#2948 = EDGE_LOOP ( 'NONE', ( #4141, #1374, #2232, #469 ) ) ;
#2949 = ADVANCED_FACE ( 'NONE', ( #5383, #6712, #2690, #2092, #7152, #2605, #4386, #3197, #4900, #1501, #381 ), #4338, .F. ) ;
#2950 = DIRECTION ( 'NONE',  ( 0.000000000000000000, 0.000000000000000000, 1.000000000000000000 ) ) ;
#2951 = VERTEX_POINT ( 'NONE', #4300 ) ;
#2952 = CARTESIAN_POINT ( 'NONE',  ( -4.000000000000000000, -2.309401076758512694, -3.433295621305382461 ) ) ;
#2953 = ORIENTED_EDGE ( 'NONE', *, *, #4305, .T. ) ;
#2954 = EDGE_CURVE ( 'NONE', #5946, #6812, #6261, .T. ) ;
#2955 = EDGE_CURVE ( 'NONE', #6476, #932, #5421, .T. ) ;
#2956 = EDGE_CURVE ( 'NONE', #2565, #1241, #5182, .T. ) ;
#2957 = FILL_AREA_STYLE_COLOUR ( '', #520 ) ;
#2958 = CARTESIAN_POINT ( 'NONE',  ( 285.0000000000000568, 8.660254037844390851, 139.9990000000000236 ) ) ;
#2959 = CONICAL_SURFACE ( 'NONE', #7173, 2.500000000000000888, 0.9599310885968785900 ) ;
#2960 = LINE ( 'NONE', #1812, #532 ) ;
#2961 = CARTESIAN_POINT ( 'NONE',  ( 164.9999999999999716, -8.660254037844389075, 140.0000000000000000 ) ) ;
#2962 = ORIENTED_EDGE ( 'NONE', *, *, #2593, .T. ) ;
#2963 = VECTOR ( 'NONE', #6309, 1000.000000000000000 ) ;
#2964 = DIRECTION ( 'NONE',  ( 0.000000000000000000, -1.000000000000000000, 0.000000000000000000 ) ) ;
#2965 = LINE ( 'NONE', #5273, #1041 ) ;
#2966 = CONTEXT_DEPENDENT_SHAPE_REPRESENTATION ( #4458, #4067 ) ;
#2967 = PLANE ( 'NONE',  #3594 ) ;
#2968 = LINE ( 'NONE', #3574, #1952 ) ;
#2969 =( NAMED_UNIT ( * ) SI_UNIT ( $, .STERADIAN. ) SOLID_ANGLE_UNIT ( ) );
#2970 = ORIENTED_EDGE ( 'NONE', *, *, #5162, .F. ) ;
#2971 = AXIS2_PLACEMENT_3D ( 'NONE', #1697, #3985, #658 ) ;
#2972 = EDGE_LOOP ( 'NONE', ( #4669, #4941, #237, #1332 ) ) ;
#2973 = PRODUCT_DEFINITION_SHAPE ( 'NONE', 'NONE',  #7374 ) ;
#2974 = ORIENTED_EDGE ( 'NONE', *, *, #3018, .F. ) ;
#2975 = DIRECTION ( 'NONE',  ( -1.000000000000000000, 0.000000000000000000, 0.000000000000000000 ) ) ;
#2976 = CARTESIAN_POINT ( 'NONE',  ( 2.500000000000000000, -2.357898499370432610, 3.252606517456513302E-15 ) ) ;
#2977 = DIRECTION ( 'NONE',  ( 0.000000000000000000, 0.000000000000000000, 1.000000000000000000 ) ) ;
#2978 = DIRECTION ( 'NONE',  ( 0.000000000000000000, 1.224646799147361589E-16, 1.000000000000000000 ) ) ;
#2979 = AXIS2_PLACEMENT_3D ( 'NONE', #2739, #1735, #4517 ) ;
#2980 = EDGE_CURVE ( 'NONE', #3497, #3960, #4904, .T. ) ;
#2981 = CARTESIAN_POINT ( 'NONE',  ( 2.500000000000000000, 2.357898499370433054, -1.951563910473907981E-15 ) ) ;
#2982 = EDGE_LOOP ( 'NONE', ( #6462, #2434, #2548 ) ) ;
#2983 = EDGE_LOOP ( 'NONE', ( #3146, #816, #3643, #6081 ) ) ;
#2984 = CIRCLE ( 'NONE', #2513, 4.000000000000000000 ) ;
#2985 = CARTESIAN_POINT ( 'NONE',  ( -2.100000000000000089, 2.571758278209441957E-16, -5.000000000000000000 ) ) ;
#2986 = ORIENTED_EDGE ( 'NONE', *, *, #6992, .T. ) ;
#2987 = ADVANCED_FACE ( 'NONE', ( #6039 ), #3281, .F. ) ;
#2988 = CIRCLE ( 'NONE', #992, 11.05000000000000071 ) ;
#2989 = CARTESIAN_POINT ( 'NONE',  ( -6.473970235329672780E-16, -4.862606272033106691, -3.745885042887442395 ) ) ;
#2990 = VECTOR ( 'NONE', #2757, 1000.000000000000000 ) ;
#2991 = EDGE_CURVE ( 'NONE', #3050, #1884, #467, .T. ) ;
#2992 = ORIENTED_EDGE ( 'NONE', *, *, #4496, .F. ) ;
#2993 = DIRECTION ( 'NONE',  ( 1.000000000000000000, 0.000000000000000000, 0.000000000000000000 ) ) ;
#2994 = AXIS2_PLACEMENT_3D ( 'NONE', #3049, #5350, #6589 ) ;
#2995 = EDGE_CURVE ( 'NONE', #1933, #4178, #401, .T. ) ;
#2996 = DIRECTION ( 'NONE',  ( 1.000000000000000000, 0.000000000000000000, 0.000000000000000000 ) ) ;
#2997 = ORIENTED_EDGE ( 'NONE', *, *, #4389, .T. ) ;
#2998 = AXIS2_PLACEMENT_3D ( 'NONE', #7053, #803, #695 ) ;
#2999 = AXIS2_PLACEMENT_3D ( 'NONE', #1647, #6501, #2858 ) ;
#3000 = VECTOR ( 'NONE', #1032, 1000.000000000000000 ) ;
#3001 = CIRCLE ( 'NONE', #3993, 2.649999999999985700 ) ;
#3002 = FACE_OUTER_BOUND ( 'NONE', #1400, .T. ) ;
#3003 = ITEM_DEFINED_TRANSFORMATION ( 'NONE', 'NONE', #3252,  #1963 ) ;
#3004 = CARTESIAN_POINT ( 'NONE',  ( -20.63749999999999929, 0.000000000000000000, 0.000000000000000000 ) ) ;
#3005 = CARTESIAN_POINT ( 'NONE',  ( -30.00000000000002842, -15.00000000000000000, 180.0000000000000284 ) ) ;
#3006 = EDGE_LOOP ( 'NONE', ( #5374, #6418, #1814, #5447 ) ) ;
#3007 = ADVANCED_FACE ( 'NONE', ( #3923, #3997 ), #4559, .T. ) ;
#3008 = CARTESIAN_POINT ( 'NONE',  ( -3.510273485745307287, -2.827716139362669967, -3.610536846335890004 ) ) ;
#3009 = VECTOR ( 'NONE', #4037, 1000.000000000000000 ) ;
#3010 = TOROIDAL_SURFACE ( 'NONE', #4956, 13.29999999999999893, 0.2000000000000027034 ) ;
#3011 = EDGE_LOOP ( 'NONE', ( #1044, #5050 ) ) ;
#3012 = VERTEX_POINT ( 'NONE', #5514 ) ;
#3013 = CARTESIAN_POINT ( 'NONE',  ( 405.0000000000000000, 8.660254037844390851, 139.9990000000000236 ) ) ;
#3014 = FACE_OUTER_BOUND ( 'NONE', #4806, .T. ) ;
#3015 =( GEOMETRIC_REPRESENTATION_CONTEXT ( 3 ) GLOBAL_UNCERTAINTY_ASSIGNED_CONTEXT ( ( #6467 ) ) GLOBAL_UNIT_ASSIGNED_CONTEXT ( ( #3830, #1106, #5150 ) ) REPRESENTATION_CONTEXT ( 'NONE', 'WORKASPACE' ) );
#3016 = CARTESIAN_POINT ( 'NONE',  ( 53.33333333333330017, -20.00000000000000000, -159.8500000000001080 ) ) ;
#3017 = DIRECTION ( 'NONE',  ( -0.000000000000000000, 1.000000000000000000, -0.000000000000000000 ) ) ;
#3018 = EDGE_CURVE ( 'NONE', #5618, #3704, #6017, .T. ) ;
#3019 = CARTESIAN_POINT ( 'NONE',  ( 53.33333333333330017, -14.99999999999999822, 165.1500000000000625 ) ) ;
#3020 = CARTESIAN_POINT ( 'NONE',  ( 303.3333333333333144, -25.00000000000000000, -159.8500000000001080 ) ) ;
#3021 = CONICAL_SURFACE ( 'NONE', #69, 2.055000000000000160, 0.7853981633974721488 ) ;
#3022 = AXIS2_PLACEMENT_3D ( 'NONE', #7150, #465, #2602 ) ;
#3023 = VECTOR ( 'NONE', #873, 1000.000000000000000 ) ;
#3024 = ORIENTED_EDGE ( 'NONE', *, *, #5965, .T. ) ;
#3025 = ORIENTED_EDGE ( 'NONE', *, *, #2575, .T. ) ;
#3026 = ITEM_DEFINED_TRANSFORMATION ( 'NONE', 'NONE', #3760,  #1963 ) ;
#3027 = FACE_OUTER_BOUND ( 'NONE', #3073, .T. ) ;
#3028 = ORIENTED_EDGE ( 'NONE', *, *, #1955, .F. ) ;
#3029 = CIRCLE ( 'NONE', #3277, 9.999999999999994671 ) ;
#3030 = AXIS2_PLACEMENT_3D ( 'NONE', #1211, #1181, #2845 ) ;
#3031 = DIRECTION ( 'NONE',  ( -1.000000000000000000, 0.000000000000000000, -0.000000000000000000 ) ) ;
#3032 = VERTEX_POINT ( 'NONE', #4479 ) ;
#3033 = EDGE_CURVE ( 'NONE', #2062, #1523, #5043, .T. ) ;
#3034 = ORIENTED_EDGE ( 'NONE', *, *, #5138, .F. ) ;
#3035 = EDGE_CURVE ( 'NONE', #76, #1288, #2666, .T. ) ;
#3036 = DIRECTION ( 'NONE',  ( 0.000000000000000000, 1.000000000000000000, 0.000000000000000000 ) ) ;
#3037 = VECTOR ( 'NONE', #6952, 1000.000000000000000 ) ;
#3038 = DIRECTION ( 'NONE',  ( 0.000000000000000000, -1.000000000000000000, 0.000000000000000000 ) ) ;
#3039 = PRODUCT_DEFINITION_SHAPE ( 'NONE', 'NONE',  #7395 ) ;
#3040 = DIRECTION ( 'NONE',  ( 1.000000000000000000, 0.000000000000000000, 0.000000000000000000 ) ) ;
#3041 =( REPRESENTATION_RELATIONSHIP ('NONE','NONE', #5587, #6025 ) REPRESENTATION_RELATIONSHIP_WITH_TRANSFORMATION ( #5274 )SHAPE_REPRESENTATION_RELATIONSHIP( ) );
#3042 = ORIENTED_EDGE ( 'NONE', *, *, #4932, .F. ) ;
#3043 = ADVANCED_FACE ( 'NONE', ( #1632 ), #4321, .F. ) ;
#3044 = CARTESIAN_POINT ( 'NONE',  ( -30.00000000000000000, 0.000000000000000000, 145.0000000000000284 ) ) ;
#3045 = PLANE ( 'NONE',  #6008 ) ;
#3046 = CARTESIAN_POINT ( 'NONE',  ( 285.0000000000000568, -8.660254037844389075, 139.9990000000000236 ) ) ;
#3047 =( NAMED_UNIT ( * ) PLANE_ANGLE_UNIT ( ) SI_UNIT ( $, .RADIAN. ) );
#3048 = ORIENTED_EDGE ( 'NONE', *, *, #6454, .T. ) ;
#3049 = CARTESIAN_POINT ( 'NONE',  ( -1.799999999999996048, 0.000000000000000000, 0.000000000000000000 ) ) ;
#3050 = VERTEX_POINT ( 'NONE', #2022 ) ;
#3051 = ORIENTED_EDGE ( 'NONE', *, *, #6846, .F. ) ;
#3052 = ADVANCED_FACE ( 'NONE', ( #3759 ), #2146, .F. ) ;
#3053 = DIRECTION ( 'NONE',  ( -0.000000000000000000, -1.000000000000000000, -0.000000000000000000 ) ) ;
#3054 = DIRECTION ( 'NONE',  ( -0.000000000000000000, 1.000000000000000000, 1.224646799147353207E-16 ) ) ;
#3055 = CARTESIAN_POINT ( 'NONE',  ( -4.000000000000000000, -2.309401076758515803, -0.4999999999999995559 ) ) ;
#3056 = CARTESIAN_POINT ( 'NONE',  ( 219.9999999999999716, -20.00000000000000000, 165.1500000000000625 ) ) ;
#3057 = CARTESIAN_POINT ( 'NONE',  ( -3.679171394226034675, -2.494631558665844739, -0.3503314178412558211 ) ) ;
#3058 = CARTESIAN_POINT ( 'NONE',  ( -6.473970235329672780E-16, -4.862606272033106691, -3.745885042887442395 ) ) ;
#3059 = VERTEX_POINT ( 'NONE', #6061 ) ;
#3060 = PRODUCT_DEFINITION_SHAPE ( 'NONE', 'NONE',  #7342 ) ;
#3061 = ITEM_DEFINED_TRANSFORMATION ( 'NONE', 'NONE', #4341,  #1963 ) ;
#3062 = ORIENTED_EDGE ( 'NONE', *, *, #3894, .T. ) ;
#3063 = CARTESIAN_POINT ( 'NONE',  ( 2.449848172108560096, 3.432307619358740514, -3.503702292528905637 ) ) ;
#3064 = ORIENTED_EDGE ( 'NONE', *, *, #717, .T. ) ;
#3065 =( NAMED_UNIT ( * ) PLANE_ANGLE_UNIT ( ) SI_UNIT ( $, .RADIAN. ) );
#3066 = DIRECTION ( 'NONE',  ( -1.000000000000000000, -0.000000000000000000, -0.000000000000000000 ) ) ;
#3067 = UNCERTAINTY_MEASURE_WITH_UNIT (LENGTH_MEASURE( 1.000000000000000082E-05 ), #7253, 'distance_accuracy_value', 'NONE');
#3068 = VERTEX_POINT ( 'NONE', #923 ) ;
#3069 = EDGE_LOOP ( 'NONE', ( #548, #4659 ) ) ;
#3070 = DIRECTION ( 'NONE',  ( -1.000000000000000000, -0.000000000000000000, -0.000000000000000000 ) ) ;
#3071 = DIRECTION ( 'NONE',  ( -0.000000000000000000, -0.000000000000000000, 1.000000000000000000 ) ) ;
#3072 = EDGE_CURVE ( 'NONE', #3960, #3899, #3839, .T. ) ;
#3073 = EDGE_LOOP ( 'NONE', ( #6676, #6251, #1384, #5488 ) ) ;
#3074 = SURFACE_STYLE_FILL_AREA ( #1781 ) ;
#3075 = EDGE_LOOP ( 'NONE', ( #4482, #2329, #739, #7082 ) ) ;
#3076 = DIRECTION ( 'NONE',  ( 0.000000000000000000, 1.000000000000000000, 0.000000000000000000 ) ) ;
#3077 = DIRECTION ( 'NONE',  ( 0.000000000000000000, -0.000000000000000000, -1.000000000000000000 ) ) ;
#3078 = FACE_BOUND ( 'NONE', #5318, .T. ) ;
#3079 =( LENGTH_UNIT ( ) NAMED_UNIT ( * ) SI_UNIT ( .MILLI., .METRE. ) );
#3080 = ORIENTED_EDGE ( 'NONE', *, *, #5380, .F. ) ;
#3081 = CARTESIAN_POINT ( 'NONE',  ( -2.000000000000001776, 0.000000000000000000, 0.000000000000000000 ) ) ;
#3082 = ADVANCED_FACE ( 'NONE', ( #2180 ), #6096, .F. ) ;
#3083 = VERTEX_POINT ( 'NONE', #1521 ) ;
#3084 = ORIENTED_EDGE ( 'NONE', *, *, #1176, .T. ) ;
#3085 = DIRECTION ( 'NONE',  ( 1.000000000000000000, 0.000000000000000000, 0.000000000000000000 ) ) ;
#3086 = PLANE ( 'NONE',  #2833 ) ;
#3087 = FACE_BOUND ( 'NONE', #3069, .T. ) ;
#3088 = DIRECTION ( 'NONE',  ( 0.000000000000000000, 0.000000000000000000, -1.000000000000000000 ) ) ;
#3089 = FACE_OUTER_BOUND ( 'NONE', #36, .T. ) ;
#3090 = CARTESIAN_POINT ( 'NONE',  ( 0.000000000000000000, 0.000000000000000000, 0.000000000000000000 ) ) ;
#3091 = ADVANCED_FACE ( 'NONE', ( #485 ), #3303, .F. ) ;
#3092 = ORIENTED_EDGE ( 'NONE', *, *, #6, .F. ) ;
#3093 = VECTOR ( 'NONE', #295, 1000.000000000000000 ) ;
#3094 = DIRECTION ( 'NONE',  ( 1.000000000000000000, 0.000000000000000000, 0.000000000000000000 ) ) ;
#3095 = ORIENTED_EDGE ( 'NONE', *, *, #3473, .F. ) ;
#3096 = CARTESIAN_POINT ( 'NONE',  ( 5.560781378645575757, 0.000000000000000000, -4.000000000000000000 ) ) ;
#3097 = ORIENTED_EDGE ( 'NONE', *, *, #5133, .F. ) ;
#3098 = VERTEX_POINT ( 'NONE', #2585 ) ;
#3099 = CARTESIAN_POINT ( 'NONE',  ( -2.000000000000000888, 12.77500000000000036, 0.000000000000000000 ) ) ;
#3100 = FACE_OUTER_BOUND ( 'NONE', #1907, .T. ) ;
#3101 = AXIS2_PLACEMENT_3D ( 'NONE', #5159, #3674, #1401 ) ;
#3102 = DIRECTION ( 'NONE',  ( -0.000000000000000000, 1.000000000000000000, -0.000000000000000000 ) ) ;
#3103 = DIRECTION ( 'NONE',  ( -1.000000000000000000, 0.000000000000000000, 0.000000000000000000 ) ) ;
#3104 = VERTEX_POINT ( 'NONE', #4882 ) ;
#3105 = ADVANCED_FACE ( 'NONE', ( #7292 ), #6861, .T. ) ;
#3106 = CARTESIAN_POINT ( 'NONE',  ( 4.197310751797292738, 0.8178363989516252985, -3.502498386812444409 ) ) ;
#3107 = CYLINDRICAL_SURFACE ( 'NONE', #1915, 2.649999999999985700 ) ;
#3108 = DIRECTION ( 'NONE',  ( -1.000000000000000000, 0.000000000000000000, 0.000000000000000000 ) ) ;
#3109 = DIRECTION ( 'NONE',  ( 6.123233995736766036E-17, -1.000000000000000000, 0.000000000000000000 ) ) ;
#3110 = ORIENTED_EDGE ( 'NONE', *, *, #1435, .T. ) ;
#3111 = CARTESIAN_POINT ( 'NONE',  ( -0.6937372685066653943, 4.453844082567723461, -3.610536846335889116 ) ) ;
#3112 = PRODUCT_DEFINITION_SHAPE ( 'NONE', 'NONE',  #7345 ) ;
#3113 = CIRCLE ( 'NONE', #6560, 0.2000000000000022593 ) ;
#3114 = VERTEX_POINT ( 'NONE', #2623 ) ;
#3115 = ORIENTED_EDGE ( 'NONE', *, *, #1364, .F. ) ;
#3116 = DIRECTION ( 'NONE',  ( -0.000000000000000000, 0.000000000000000000, -1.000000000000000000 ) ) ;
#3117 = CARTESIAN_POINT ( 'NONE',  ( 435.0000000000000568, -8.660254037844389075, 139.9990000000000236 ) ) ;
#3118 = DIRECTION ( 'NONE',  ( 1.000000000000000000, 0.000000000000000000, 0.000000000000000000 ) ) ;
#3119 = CARTESIAN_POINT ( 'NONE',  ( -4.000000000000000000, 2.309401076758498483, -0.4999999999999927280 ) ) ;
#3120 = EDGE_CURVE ( 'NONE', #5618, #5368, #3833, .T. ) ;
#3121 = VECTOR ( 'NONE', #3076, 1000.000000000000000 ) ;
#3122 = AXIS2_PLACEMENT_3D ( 'NONE', #3310, #1116, #7262 ) ;
#3123 = CIRCLE ( 'NONE', #6872, 2.649999999999985700 ) ;
#3124 = VECTOR ( 'NONE', #359, 1000.000000000000000 ) ;
#3125 = CIRCLE ( 'NONE', #1359, 9.999999999999998224 ) ;
#3126 = MANIFOLD_SOLID_BREP ( 'Mirror1', #3382 ) ;
#3127 = CARTESIAN_POINT ( 'NONE',  ( 325.0000000000000000, 8.660254037844390851, 140.0000000000000000 ) ) ;
#3128 = DIRECTION ( 'NONE',  ( 0.000000000000000000, 0.000000000000000000, 1.000000000000000000 ) ) ;
#3129 = VERTEX_POINT ( 'NONE', #101 ) ;
#3130 = AXIS2_PLACEMENT_3D ( 'NONE', #6976, #2389, #5853 ) ;
#3131 =( GEOMETRIC_REPRESENTATION_CONTEXT ( 3 ) GLOBAL_UNCERTAINTY_ASSIGNED_CONTEXT ( ( #3600 ) ) GLOBAL_UNIT_ASSIGNED_CONTEXT ( ( #4741, #1190, #1773 ) ) REPRESENTATION_CONTEXT ( 'NONE', 'WORKASPACE' ) );
#3132 = FACE_BOUND ( 'NONE', #3568, .T. ) ;
#3133 = DIRECTION ( 'NONE',  ( 1.000000000000000000, 0.000000000000000000, 0.000000000000000000 ) ) ;
#3134 = ORIENTED_EDGE ( 'NONE', *, *, #6128, .F. ) ;
#3135 = CARTESIAN_POINT ( 'NONE',  ( 405.0000000000000000, 8.660254037844390851, 145.0000000000000284 ) ) ;
#3136 = ADVANCED_FACE ( 'NONE', ( #4655 ), #4365, .F. ) ;
#3137 =( REPRESENTATION_RELATIONSHIP ('NONE','NONE', #5587, #1193 ) REPRESENTATION_RELATIONSHIP_WITH_TRANSFORMATION ( #4508 )SHAPE_REPRESENTATION_RELATIONSHIP( ) );
#3138 = VECTOR ( 'NONE', #6201, 1000.000000000000000 ) ;
#3139 = CARTESIAN_POINT ( 'NONE',  ( -5.000000000000000888, -8.660254037844389075, 145.0000000000000284 ) ) ;
#3140 = AXIS2_PLACEMENT_3D ( 'NONE', #3691, #4898, #6587 ) ;
#3141 = EDGE_CURVE ( 'NONE', #3817, #2951, #6845, .T. ) ;
#3142 = LINE ( 'NONE', #4970, #4246 ) ;
#3143 = ORIENTED_EDGE ( 'NONE', *, *, #2154, .T. ) ;
#3144 = DIRECTION ( 'NONE',  ( 0.000000000000000000, 0.000000000000000000, -1.000000000000000000 ) ) ;
#3145 = VECTOR ( 'NONE', #2479, 1000.000000000000000 ) ;
#3146 = ORIENTED_EDGE ( 'NONE', *, *, #4343, .F. ) ;
#3147 = DIRECTION ( 'NONE',  ( -0.7071067811865306973, 8.659560562355138702E-17, -0.7071067811865643371 ) ) ;
#3148 = CARTESIAN_POINT ( 'NONE',  ( 1.567478505476134606E-15, 4.618802153517012066, -3.433295621305382905 ) ) ;
#3149 = DIRECTION ( 'NONE',  ( 0.000000000000000000, 0.000000000000000000, 1.000000000000000000 ) ) ;
#3150 = AXIS2_PLACEMENT_3D ( 'NONE', #2624, #1989, #6063 ) ;
#3151 = ORIENTED_EDGE ( 'NONE', *, *, #4101, .T. ) ;
#3152 = EDGE_CURVE ( 'NONE', #630, #1550, #5065, .T. ) ;
#3153 = CARTESIAN_POINT ( 'NONE',  ( 75.00000000000001421, 8.660254037844390851, 145.0000000000000284 ) ) ;
#3154 = ITEM_DEFINED_TRANSFORMATION ( 'NONE', 'NONE', #2888,  #1963 ) ;
#3155 = CARTESIAN_POINT ( 'NONE',  ( -2.500000000000000444, 3.061616997868383634E-16, -25.03750572909317285 ) ) ;
#3156 = PLANE ( 'NONE',  #6399 ) ;
#3157 = DIRECTION ( 'NONE',  ( 6.123233995736766036E-17, -1.000000000000000000, 0.000000000000000000 ) ) ;
#3158 = VERTEX_POINT ( 'NONE', #6884 ) ;
#3159 = LINE ( 'NONE', #825, #4092 ) ;
#3160 = ORIENTED_EDGE ( 'NONE', *, *, #1783, .T. ) ;
#3161 = EDGE_LOOP ( 'NONE', ( #6505, #1614 ) ) ;
#3162 = LINE ( 'NONE', #5462, #23 ) ;
#3163 = CARTESIAN_POINT ( 'NONE',  ( 4.000000000000000000, 0.3987449864460005378, -0.01220643443059817035 ) ) ;
#3164 = DIRECTION ( 'NONE',  ( 0.000000000000000000, 1.000000000000000000, 0.000000000000000000 ) ) ;
#3165 = LINE ( 'NONE', #7279, #3500 ) ;
#3166 = LINE ( 'NONE', #1621, #5540 ) ;
#3167 = CARTESIAN_POINT ( 'NONE',  ( 0.000000000000000000, 0.000000000000000000, -140.0000000000000000 ) ) ;
#3168 = EDGE_CURVE ( 'NONE', #3238, #2887, #6917, .T. ) ;
#3169 = CARTESIAN_POINT ( 'NONE',  ( -6.259644161404860030E-16, -4.618802153517027165, -3.433295621305388234 ) ) ;
#3170 = ORIENTED_EDGE ( 'NONE', *, *, #5009, .F. ) ;
#3171 = CARTESIAN_POINT ( 'NONE',  ( 3.679171394226031122, 2.494631558665830973, -0.3503314178412474389 ) ) ;
#3172 = DIRECTION ( 'NONE',  ( -1.000000000000000000, -0.000000000000000000, -0.000000000000000000 ) ) ;
#3173 = ORIENTED_EDGE ( 'NONE', *, *, #5313, .F. ) ;
#3174 = DIRECTION ( 'NONE',  ( -0.000000000000000000, 1.000000000000000000, -0.000000000000000000 ) ) ;
#3175 =( NAMED_UNIT ( * ) SI_UNIT ( $, .STERADIAN. ) SOLID_ANGLE_UNIT ( ) );
#3176 = CARTESIAN_POINT ( 'NONE',  ( 195.0000000000000000, 8.660254037844390851, 139.9990000000000236 ) ) ;
#3177 = CARTESIAN_POINT ( 'NONE',  ( -1.999999999999998224, 0.000000000000000000, 0.000000000000000000 ) ) ;
#3178 = ADVANCED_FACE ( 'NONE', ( #4053 ), #3918, .T. ) ;
#3179 = EDGE_LOOP ( 'NONE', ( #3199, #5535, #527, #5223 ) ) ;
#3180 = CARTESIAN_POINT ( 'NONE',  ( 320.0000000000000000, 0.000000000000000000, 123.0000000000000000 ) ) ;
#3181 = ORIENTED_EDGE ( 'NONE', *, *, #6862, .F. ) ;
#3182 = PRODUCT_DEFINITION_SHAPE ( 'NONE', 'NONE',  #7351 ) ;
#3183 = LINE ( 'NONE', #335, #1618 ) ;
#3184 = DIRECTION ( 'NONE',  ( 0.000000000000000000, 0.000000000000000000, 1.000000000000000000 ) ) ;
#3185 = DIRECTION ( 'NONE',  ( 0.000000000000000000, 1.000000000000000000, -1.287488025362403787E-15 ) ) ;
#3186 = EDGE_CURVE ( 'NONE', #6064, #1325, #5637, .T. ) ;
#3187 = ORIENTED_EDGE ( 'NONE', *, *, #6006, .F. ) ;
#3188 = LINE ( 'NONE', #4294, #1112 ) ;
#3189 = MANIFOLD_SOLID_BREP ( 'M5 Clearance Hole1', #3615 ) ;
#3190 = B_SPLINE_CURVE_WITH_KNOTS ( 'NONE', 3,
 ( #3055, #3630, #7085, #2388, #1426, #208 ),
 .UNSPECIFIED., .F., .F.,
 ( 4, 2, 4 ),
 ( 0.003358874760055550156, 0.004541967308452096383, 0.005725059856848641743 ),
 .UNSPECIFIED. ) ;
#3191 = ITEM_DEFINED_TRANSFORMATION ( 'NONE', 'NONE', #4595,  #1963 ) ;
#3192 = CARTESIAN_POINT ( 'NONE',  ( 4.999999999999999112, -8.660254037844389075, 139.9990000000000236 ) ) ;
#3193 = CARTESIAN_POINT ( 'NONE',  ( -30.00000000000002842, -25.00000000000000000, 200.0000000000000000 ) ) ;
#3194 = DIRECTION ( 'NONE',  ( 0.000000000000000000, 0.000000000000000000, 1.000000000000000000 ) ) ;
#3195 = PRODUCT_DEFINITION ( 'UNKNOWN', '', #5539, #3735 ) ;
#3196 = ORIENTED_EDGE ( 'NONE', *, *, #1455, .T. ) ;
#3197 = FACE_BOUND ( 'NONE', #4007, .T. ) ;
#3198 = VERTEX_POINT ( 'NONE', #1740 ) ;
#3199 = ORIENTED_EDGE ( 'NONE', *, *, #7244, .T. ) ;
#3200 = CARTESIAN_POINT ( 'NONE',  ( 4.000000000000000000, -2.309401076758516691, -0.4999999999999995559 ) ) ;
#3201 = CARTESIAN_POINT ( 'NONE',  ( 0.6810597143197052450, 4.461075778259290914, -3.598441714920602053 ) ) ;
#3202 = DIRECTION ( 'NONE',  ( 0.000000000000000000, 0.000000000000000000, -1.000000000000000000 ) ) ;
#3203 = DIRECTION ( 'NONE',  ( 1.000000000000000000, 0.000000000000000000, 0.000000000000000000 ) ) ;
#3204 = DIRECTION ( 'NONE',  ( 0.000000000000000000, 1.000000000000000000, 0.000000000000000000 ) ) ;
#3205 = CARTESIAN_POINT ( 'NONE',  ( 75.00000000000001421, 8.660254037844390851, 139.9990000000000236 ) ) ;
#3206 = VERTEX_POINT ( 'NONE', #1216 ) ;
#3207 = CARTESIAN_POINT ( 'NONE',  ( 355.0000000000000000, 8.660254037844390851, 139.9990000000000236 ) ) ;
#3208 = DIRECTION ( 'NONE',  ( -0.000000000000000000, 1.000000000000000000, -0.000000000000000000 ) ) ;
#3209 = EDGE_CURVE ( 'NONE', #4692, #4184, #5221, .T. ) ;
#3210 = DIRECTION ( 'NONE',  ( -0.000000000000000000, 1.000000000000000000, -0.000000000000000000 ) ) ;
#3211 = AXIS2_PLACEMENT_3D ( 'NONE', #5139, #2764, #3975 ) ;
#3212 = SURFACE_STYLE_FILL_AREA ( #448 ) ;
#3213 = CARTESIAN_POINT ( 'NONE',  ( 5.000000000000004441, 5.204748896376250699E-16, -4.250000000000000000 ) ) ;
#3214 = AXIS2_PLACEMENT_3D ( 'NONE', #5632, #2478, #3646 ) ;
#3215 = AXIS2_PLACEMENT_3D ( 'NONE', #225, #1267, #4145 ) ;
#3216 = ORIENTED_EDGE ( 'NONE', *, *, #6455, .T. ) ;
#3217 = VERTEX_POINT ( 'NONE', #5183 ) ;
#3218 = DIRECTION ( 'NONE',  ( 0.000000000000000000, 0.000000000000000000, -1.000000000000000000 ) ) ;
#3219 = ORIENTED_EDGE ( 'NONE', *, *, #5476, .F. ) ;
#3220 = LINE ( 'NONE', #5981, #4724 ) ;
#3221 = VECTOR ( 'NONE', #1309, 1000.000000000000114 ) ;
#3222 = EDGE_CURVE ( 'NONE', #7, #4634, #461, .T. ) ;
#3223 = EDGE_CURVE ( 'NONE', #732, #7234, #2327, .T. ) ;
#3224 = DIRECTION ( 'NONE',  ( 0.000000000000000000, -1.000000000000000000, 0.000000000000000000 ) ) ;
#3225 = DIRECTION ( 'NONE',  ( 0.000000000000000000, 0.000000000000000000, -1.000000000000000000 ) ) ;
#3226 = ORIENTED_EDGE ( 'NONE', *, *, #2628, .T. ) ;
#3227 = CIRCLE ( 'NONE', #6604, 0.2000000000000000944 ) ;
#3228 = CYLINDRICAL_SURFACE ( 'NONE', #6608, 10.72500000000000142 ) ;
#3229 = CONTEXT_DEPENDENT_SHAPE_REPRESENTATION ( #4990, #2384 ) ;
#3230 = CARTESIAN_POINT ( 'NONE',  ( 25.00000000000000000, 2.055000000000000160, 0.000000000000000000 ) ) ;
#3231 = FACE_BOUND ( 'NONE', #3433, .T. ) ;
#3232 = EDGE_CURVE ( 'NONE', #5434, #6352, #4697, .T. ) ;
#3233 = DIRECTION ( 'NONE',  ( 0.000000000000000000, 0.000000000000000000, 1.000000000000000000 ) ) ;
#3234 = VERTEX_POINT ( 'NONE', #242 ) ;
#3235 = DIRECTION ( 'NONE',  ( 1.000000000000000000, 0.000000000000000000, 0.000000000000000000 ) ) ;
#3236 = VECTOR ( 'NONE', #4869, 1000.000000000000000 ) ;
#3237 = ORIENTED_EDGE ( 'NONE', *, *, #1373, .F. ) ;
#3238 = VERTEX_POINT ( 'NONE', #7022 ) ;
#3239 = PLANE ( 'NONE',  #3706 ) ;
#3240 = DIRECTION ( 'NONE',  ( 0.000000000000000000, 0.000000000000000000, -1.000000000000000000 ) ) ;
#3241 = ITEM_DEFINED_TRANSFORMATION ( 'NONE', 'NONE', #6047,  #1963 ) ;
#3242 = CARTESIAN_POINT ( 'NONE',  ( 2.687328764639642653, -3.067272167851299969, -0.05923475698271395140 ) ) ;
#3243 = DIRECTION ( 'NONE',  ( 0.000000000000000000, -1.000000000000000000, 0.000000000000000000 ) ) ;
#3244 = AXIS2_PLACEMENT_3D ( 'NONE', #4185, #5846, #5960 ) ;
#3245 = DIRECTION ( 'NONE',  ( -0.000000000000000000, 1.000000000000000000, -0.000000000000000000 ) ) ;
#3246 = PLANE ( 'NONE',  #1353 ) ;
#3247 = ORIENTED_EDGE ( 'NONE', *, *, #2033, .T. ) ;
#3248 = EDGE_CURVE ( 'NONE', #6476, #1413, #1354, .T. ) ;
#3249 = CARTESIAN_POINT ( 'NONE',  ( 355.0000000000000000, 8.660254037844390851, 139.9990000000000236 ) ) ;
#3250 = VECTOR ( 'NONE', #3549, 1000.000000000000000 ) ;
#3251 = DIRECTION ( 'NONE',  ( 0.000000000000000000, 1.000000000000000000, 0.000000000000000000 ) ) ;
#3252 = AXIS2_PLACEMENT_3D ( 'NONE', #5014, #4926, #7295 ) ;
#3253 = CIRCLE ( 'NONE', #539, 2.649999999999985700 ) ;
#3254 = FACE_OUTER_BOUND ( 'NONE', #406, .T. ) ;
#3255 = CARTESIAN_POINT ( 'NONE',  ( 5.000000000000000888, 0.000000000000000000, 0.000000000000000000 ) ) ;
#3256 = VECTOR ( 'NONE', #5592, 1000.000000000000000 ) ;
#3257 = FILL_AREA_STYLE_COLOUR ( '', #4962 ) ;
#3258 = DIRECTION ( 'NONE',  ( -1.000000000000000000, -0.000000000000000000, -0.000000000000000000 ) ) ;
#3259 = AXIS2_PLACEMENT_3D ( 'NONE', #4309, #4395, #6161 ) ;
#3260 = ORIENTED_EDGE ( 'NONE', *, *, #5695, .F. ) ;
#3261 = VERTEX_POINT ( 'NONE', #5327 ) ;
#3262 = CARTESIAN_POINT ( 'NONE',  ( 400.0000000000000000, 0.000000000000000000, 0.000000000000000000 ) ) ;
#3263 = ORIENTED_EDGE ( 'NONE', *, *, #7216, .T. ) ;
#3264 = AXIS2_PLACEMENT_3D ( 'NONE', #2685, #851, #6075 ) ;
#3265 = MECHANICAL_DESIGN_GEOMETRIC_PRESENTATION_REPRESENTATION (  '', ( #547 ), #2316 ) ;
#3266 = CARTESIAN_POINT ( 'NONE',  ( 386.6666666666666288, -14.99999999999999822, 165.1500000000000625 ) ) ;
#3267 = CARTESIAN_POINT ( 'NONE',  ( 219.9999999999999716, -20.00000000000000000, 165.1500000000000625 ) ) ;
#3268 = DIRECTION ( 'NONE',  ( 1.000000000000000000, 0.000000000000000000, 0.000000000000000000 ) ) ;
#3269 = ADVANCED_FACE ( 'NONE', ( #4764 ), #6384, .F. ) ;
#3270 = SHAPE_REPRESENTATION ( 'side rail', ( #1963 ), #5422 ) ;
#3271 = CONICAL_SURFACE ( 'NONE', #3264, 4.000000000000000000, 0.8911886515913786111 ) ;
#3272 = EDGE_LOOP ( 'NONE', ( #5025, #3260, #6298, #591 ) ) ;
#3273 = EDGE_CURVE ( 'NONE', #1780, #4157, #1249, .T. ) ;
#3274 = FACE_OUTER_BOUND ( 'NONE', #107, .T. ) ;
#3275 = PLANE ( 'NONE',  #4327 ) ;
#3276 = CARTESIAN_POINT ( 'NONE',  ( 275.0000000000000000, -8.660254037844389075, 145.0000000000000284 ) ) ;
#3277 = AXIS2_PLACEMENT_3D ( 'NONE', #1992, #4978, #1372 ) ;
#3278 = DIRECTION ( 'NONE',  ( 6.123233995736766036E-17, -1.000000000000000000, 0.000000000000000000 ) ) ;
#3279 = VECTOR ( 'NONE', #5818, 1000.000000000000000 ) ;
#3280 = VERTEX_POINT ( 'NONE', #4796 ) ;
#3281 = PLANE ( 'NONE',  #5408 ) ;
#3282 = B_SPLINE_CURVE_WITH_KNOTS ( 'NONE', 3,
 ( #3874, #2741, #995, #5598, #5561, #5041, #445, #2776 ),
 .UNSPECIFIED., .F., .F.,
 ( 4, 2, 2, 4 ),
 ( 2.465131517390770070E-07, 0.001183067374689869946, 0.001774477805458935659, 0.002365888236228001588 ),
 .UNSPECIFIED. ) ;
#3283 = EDGE_CURVE ( 'NONE', #541, #450, #5901, .T. ) ;
#3284 = EDGE_LOOP ( 'NONE', ( #6510, #3781, #2296, #1916, #2871, #4864 ) ) ;
#3285 = ORIENTED_EDGE ( 'NONE', *, *, #3141, .F. ) ;
#3286 = FACE_OUTER_BOUND ( 'NONE', #1237, .T. ) ;
#3287 = CIRCLE ( 'NONE', #4250, 2.649999999999985700 ) ;
#3288 = PLANE ( 'NONE',  #1506 ) ;
#3289 = CARTESIAN_POINT ( 'NONE',  ( 75.00000000000001421, 8.660254037844390851, 139.9990000000000236 ) ) ;
#3290 = DIRECTION ( 'NONE',  ( -1.000000000000000000, 0.000000000000000000, 0.000000000000000000 ) ) ;
#3291 = DIRECTION ( 'NONE',  ( 1.000000000000000000, 0.000000000000000000, 0.000000000000000000 ) ) ;
#3292 = UNCERTAINTY_MEASURE_WITH_UNIT (LENGTH_MEASURE( 1.000000000000000082E-05 ), #1555, 'distance_accuracy_value', 'NONE');
#3293 = CARTESIAN_POINT ( 'NONE',  ( -5.000000000000000888, 8.660254037844390851, 140.0000000000000000 ) ) ;
#3294 = VECTOR ( 'NONE', #6670, 1000.000000000000000 ) ;
#3295 =( REPRESENTATION_RELATIONSHIP ('NONE','NONE', #5587, #5294 ) REPRESENTATION_RELATIONSHIP_WITH_TRANSFORMATION ( #1336 )SHAPE_REPRESENTATION_RELATIONSHIP( ) );
#3296 = ADVANCED_FACE ( 'NONE', ( #3089 ), #2946, .T. ) ;
#3297 = ORIENTED_EDGE ( 'NONE', *, *, #4714, .T. ) ;
#3298 = CARTESIAN_POINT ( 'NONE',  ( -0.2277608394786177770, 0.000000000000000000, 0.000000000000000000 ) ) ;
#3299 = CARTESIAN_POINT ( 'NONE',  ( -10.00000000000000000, 0.000000000000000000, 140.0000000000000000 ) ) ;
#3300 = CARTESIAN_POINT ( 'NONE',  ( 365.0000000000000000, 8.660254037844390851, 140.0000000000000000 ) ) ;
#3301 = CARTESIAN_POINT ( 'NONE',  ( 0.2277608394786177770, 1.419059478511995659E-15, -10.72500000000000142 ) ) ;
#3302 = FILL_AREA_STYLE_COLOUR ( '', #1834 ) ;
#3303 = PLANE ( 'NONE',  #1343 ) ;
#3304 = PRODUCT_DEFINITION ( 'UNKNOWN', '', #762, #3909 ) ;
#3305 = PRESENTATION_LAYER_ASSIGNMENT (  '', '', ( #6545 ) ) ;
#3306 = EDGE_LOOP ( 'NONE', ( #3556, #4286, #1526, #6324 ) ) ;
#3307 = EDGE_LOOP ( 'NONE', ( #1209, #2457, #1702, #2819 ) ) ;
#3308 = CARTESIAN_POINT ( 'NONE',  ( 386.6666666666666288, -30.00000000000000355, -162.5000000000000853 ) ) ;
#3309 = VERTEX_POINT ( 'NONE', #3667 ) ;
#3310 = CARTESIAN_POINT ( 'NONE',  ( 136.6666666666666288, -20.00000000000000000, -162.5000000000000853 ) ) ;
#3311 = FACE_OUTER_BOUND ( 'NONE', #270, .T. ) ;
#3312 = CARTESIAN_POINT ( 'NONE',  ( 303.3333333333333144, -14.99999999999999822, 159.8500000000001080 ) ) ;
#3313 = ORIENTED_EDGE ( 'NONE', *, *, #2907, .T. ) ;
#3314 = CARTESIAN_POINT ( 'NONE',  ( 0.000000000000000000, 0.000000000000000000, -4.974599999999998801 ) ) ;
#3315 = SHAPE_DEFINITION_REPRESENTATION ( #1929, #3270 ) ;
#3316 = EDGE_CURVE ( 'NONE', #1241, #5950, #6177, .T. ) ;
#3317 = CONTEXT_DEPENDENT_SHAPE_REPRESENTATION ( #5354, #2923 ) ;
#3318 = LINE ( 'NONE', #9, #1957 ) ;
#3319 = DIRECTION ( 'NONE',  ( 1.000000000000000000, 0.000000000000000000, 0.000000000000000000 ) ) ;
#3320 = ORIENTED_EDGE ( 'NONE', *, *, #6837, .F. ) ;
#3321 = CARTESIAN_POINT ( 'NONE',  ( -0.7826237921249277196, 0.000000000000000000, 0.000000000000000000 ) ) ;
#3322 = EDGE_LOOP ( 'NONE', ( #4825, #5952, #1170, #2682 ) ) ;
#3323 = ORIENTED_EDGE ( 'NONE', *, *, #2691, .T. ) ;
#3324 = CARTESIAN_POINT ( 'NONE',  ( 4.197393957002303999, 7.772902908466098641E-14, -3.503767560748929810 ) ) ;
#3325 = CARTESIAN_POINT ( 'NONE',  ( 4.175002511812151873, 2.208363329454889445, -3.469254087858244073 ) ) ;
#3326 = CONTEXT_DEPENDENT_SHAPE_REPRESENTATION ( #860, #82 ) ;
#3327 = CARTESIAN_POINT ( 'NONE',  ( 386.6666666666666288, -20.00000000000000000, 165.1500000000000625 ) ) ;
#3328 = CARTESIAN_POINT ( 'NONE',  ( 1.799999999999996048, 0.000000000000000000, 0.000000000000000000 ) ) ;
#3329 = EDGE_CURVE ( 'NONE', #3602, #6275, #3611, .T. ) ;
#3330 = PLANE ( 'NONE',  #1125 ) ;
#3331 = DIRECTION ( 'NONE',  ( 0.000000000000000000, 0.000000000000000000, -1.000000000000000000 ) ) ;
#3332 = EDGE_CURVE ( 'NONE', #4483, #841, #1122, .T. ) ;
#3333 = VERTEX_POINT ( 'NONE', #4690 ) ;
#3334 = DIRECTION ( 'NONE',  ( 0.000000000000000000, 0.000000000000000000, 1.000000000000000000 ) ) ;
#3335 = DIRECTION ( 'NONE',  ( -0.000000000000000000, -0.000000000000000000, -1.000000000000000000 ) ) ;
#3336 = CARTESIAN_POINT ( 'NONE',  ( -4.999999999999997335, -8.660254037844389075, 140.0000000000000000 ) ) ;
#3337 = DIRECTION ( 'NONE',  ( 0.000000000000000000, 0.000000000000000000, 1.000000000000000000 ) ) ;
#3338 = EDGE_CURVE ( 'NONE', #3638, #4072, #410, .T. ) ;
#3339 = DIRECTION ( 'NONE',  ( 1.000000000000000000, 0.000000000000000000, 0.000000000000000000 ) ) ;
#3340 = ORIENTED_EDGE ( 'NONE', *, *, #5545, .T. ) ;
#3341 = EDGE_CURVE ( 'NONE', #4268, #1111, #5360, .T. ) ;
#3342 = EDGE_LOOP ( 'NONE', ( #761, #2357 ) ) ;
#3343 = VECTOR ( 'NONE', #2804, 1000.000000000000000 ) ;
#3344 = APPLICATION_PROTOCOL_DEFINITION ( 'draft international standard', 'automotive_design', 1998, #4775 ) ;
#3345 = EDGE_LOOP ( 'NONE', ( #736, #1077, #6071, #3173 ) ) ;
#3346 = FACE_OUTER_BOUND ( 'NONE', #837, .T. ) ;
#3347 = VECTOR ( 'NONE', #65, 1000.000000000000000 ) ;
#3348 = CARTESIAN_POINT ( 'NONE',  ( 205.0000000000000284, 8.660254037844390851, 139.9990000000000236 ) ) ;
#3349 = VERTEX_POINT ( 'NONE', #3554 ) ;
#3350 = CARTESIAN_POINT ( 'NONE',  ( 13.50000000000000000, 0.000000000000000000, 125.0000000000000000 ) ) ;
#3351 = AXIS2_PLACEMENT_3D ( 'NONE', #5322, #97, #3515 ) ;
#3352 = DIRECTION ( 'NONE',  ( 0.000000000000000000, -1.000000000000000000, 0.000000000000000000 ) ) ;
#3353 = CARTESIAN_POINT ( 'NONE',  ( 303.3333333333333144, -20.00000000000000000, -165.1500000000000625 ) ) ;
#3354 = CARTESIAN_POINT ( 'NONE',  ( 219.9999999999999716, -30.00000000000000355, -162.5000000000000853 ) ) ;
#3355 = ORIENTED_EDGE ( 'NONE', *, *, #4235, .T. ) ;
#3356 = DIRECTION ( 'NONE',  ( 0.000000000000000000, -1.000000000000000000, 0.000000000000000000 ) ) ;
#3357 = ADVANCED_FACE ( 'NONE', ( #4833 ), #6456, .F. ) ;
#3358 = EDGE_LOOP ( 'NONE', ( #5719, #1880 ) ) ;
#3359 = ORIENTED_EDGE ( 'NONE', *, *, #638, .F. ) ;
#3360 = FACE_BOUND ( 'NONE', #3011, .T. ) ;
#3361 = CARTESIAN_POINT ( 'NONE',  ( 303.3333333333333144, -20.00000000000000000, 165.1500000000000625 ) ) ;
#3362 = CONTEXT_DEPENDENT_SHAPE_REPRESENTATION ( #5844, #4943 ) ;
#3363 = CARTESIAN_POINT ( 'NONE',  ( 4.000000000000000000, -2.309401076758514915, -5.000000000000000000 ) ) ;
#3364 = DIRECTION ( 'NONE',  ( 0.000000000000000000, 0.000000000000000000, -1.000000000000000000 ) ) ;
#3365 = VERTEX_POINT ( 'NONE', #2981 ) ;
#3366 = CARTESIAN_POINT ( 'NONE',  ( 4.999999999999999112, 8.660254037844390851, 150.0000000000000000 ) ) ;
#3367 = AXIS2_PLACEMENT_3D ( 'NONE', #1817, #2482, #6337 ) ;
#3368 = ADVANCED_FACE ( 'NONE', ( #1394 ), #5287, .F. ) ;
#3369 = EDGE_LOOP ( 'NONE', ( #4610, #6448, #2269 ) ) ;
#3370 = EDGE_CURVE ( 'NONE', #3365, #2423, #1797, .T. ) ;
#3371 = DIRECTION ( 'NONE',  ( -1.000000000000000000, 0.000000000000000000, 0.000000000000000000 ) ) ;
#3372 = LINE ( 'NONE', #444, #3766 ) ;
#3373 = CARTESIAN_POINT ( 'NONE',  ( 4.000000000000000000, -2.309401076758514915, -3.433295621305383349 ) ) ;
#3374 = CARTESIAN_POINT ( 'NONE',  ( 386.6666666666666288, -15.00000000000000000, 162.5000000000000853 ) ) ;
#3375 = AXIS2_PLACEMENT_3D ( 'NONE', #267, #7116, #6677 ) ;
#3376 = FILL_AREA_STYLE_COLOUR ( '', #7337 ) ;
#3377 = VERTEX_POINT ( 'NONE', #3019 ) ;
#3378=STYLED_ITEM('',(#7425),#3189);
#3379 = AXIS2_PLACEMENT_3D ( 'NONE', #2127, #6150, #1418 ) ;
#3380 = ORIENTED_EDGE ( 'NONE', *, *, #3560, .F. ) ;
#3381 = EDGE_CURVE ( 'NONE', #4934, #5816, #6095, .T. ) ;
#3382 = CLOSED_SHELL ( 'NONE', ( #7339, #145, #2743, #4663, #902, #4587, #2829, #2332, #78, #5151, #3724, #3467 ) ) ;
#3383 = CARTESIAN_POINT ( 'NONE',  ( 280.0000000000000000, 0.000000000000000000, -123.0000000000000000 ) ) ;
#3384 = ORIENTED_EDGE ( 'NONE', *, *, #4721, .F. ) ;
#3385 = DIRECTION ( 'NONE',  ( 1.000000000000000000, 0.000000000000000000, 0.000000000000000000 ) ) ;
#3386 = VERTEX_POINT ( 'NONE', #6817 ) ;
#3387 = VECTOR ( 'NONE', #5001, 1000.000000000000114 ) ;
#3388 = CARTESIAN_POINT ( 'NONE',  ( 0.6937372685066666156, -4.453844082567737672, -3.610536846335894445 ) ) ;
#3389 = ORIENTED_EDGE ( 'NONE', *, *, #4516, .F. ) ;
#3390 = EDGE_CURVE ( 'NONE', #3365, #977, #240, .T. ) ;
#3391 = AXIS2_PLACEMENT_3D ( 'NONE', #6425, #4129, #2533 ) ;
#3392 = STYLED_ITEM ( 'NONE', ( #2708 ), #2710 ) ;
#3393 = CIRCLE ( 'NONE', #5911, 11.05000000000000071 ) ;
#3394 = FACE_BOUND ( 'NONE', #3889, .T. ) ;
#3395 = DIRECTION ( 'NONE',  ( 1.000000000000000000, 0.000000000000000000, 0.000000000000000000 ) ) ;
#3396 = DIRECTION ( 'NONE',  ( 0.000000000000000000, 0.000000000000000000, 1.000000000000000000 ) ) ;
#3397 = VERTEX_POINT ( 'NONE', #4686 ) ;
#3398 = AXIS2_PLACEMENT_3D ( 'NONE', #3328, #5143, #3364 ) ;
#3399 = CARTESIAN_POINT ( 'NONE',  ( 2.500000000000000444, 0.000000000000000000, -5.000000000000000888 ) ) ;
#3400 = AXIS2_PLACEMENT_3D ( 'NONE', #7334, #2748, #5521 ) ;
#3401 = EDGE_CURVE ( 'NONE', #4768, #1782, #6424, .T. ) ;
#3402 = ORIENTED_EDGE ( 'NONE', *, *, #7125, .T. ) ;
#3403 = CARTESIAN_POINT ( 'NONE',  ( 275.0000000000000000, 8.660254037844390851, 145.0000000000000284 ) ) ;
#3404 = DIRECTION ( 'NONE',  ( -0.000000000000000000, 0.000000000000000000, 1.000000000000000000 ) ) ;
#3405 = VECTOR ( 'NONE', #1165, 1000.000000000000000 ) ;
#3406 = CYLINDRICAL_SURFACE ( 'NONE', #4924, 13.50000000000000000 ) ;
#3407 = DIRECTION ( 'NONE',  ( 1.000000000000000000, 0.000000000000000000, 0.000000000000000000 ) ) ;
#3408 = AXIS2_PLACEMENT_3D ( 'NONE', #3761, #7137, #5367 ) ;
#3409 = ORIENTED_EDGE ( 'NONE', *, *, #4152, .T. ) ;
#3410 = CARTESIAN_POINT ( 'NONE',  ( 195.0000000000000000, -8.660254037844389075, 139.9990000000000236 ) ) ;
#3411 = EDGE_LOOP ( 'NONE', ( #704, #5064, #1024, #1991 ) ) ;
#3412 = VECTOR ( 'NONE', #1203, 1000.000000000000000 ) ;
#3413 = PRODUCT_DEFINITION_SHAPE ( 'NONE', 'NONE',  #7404 ) ;
#3414 = FACE_BOUND ( 'NONE', #6937, .T. ) ;
#3415 = CARTESIAN_POINT ( 'NONE',  ( -0.5469614295416921346, 4.303013824936271270, -3.535263753543735454 ) ) ;
#3416 = DIRECTION ( 'NONE',  ( 0.000000000000000000, 0.000000000000000000, 1.000000000000000000 ) ) ;
#3417 = CARTESIAN_POINT ( 'NONE',  ( 53.33333333333330017, -20.00000000000000000, -159.8500000000001080 ) ) ;
#3418 = EDGE_CURVE ( 'NONE', #1782, #5777, #4730, .T. ) ;
#3419 = VECTOR ( 'NONE', #2753, 1000.000000000000000 ) ;
#3420 =( LENGTH_UNIT ( ) NAMED_UNIT ( * ) SI_UNIT ( .MILLI., .METRE. ) );
#3421 = ORIENTED_EDGE ( 'NONE', *, *, #7080, .F. ) ;
#3423 = VECTOR ( 'NONE', #4367, 1000.000000000000000 ) ;
#3422 =( NAMED_UNIT ( * ) SI_UNIT ( $, .STERADIAN. ) SOLID_ANGLE_UNIT ( ) );
#3424 = ORIENTED_EDGE ( 'NONE', *, *, #6574, .F. ) ;
#3425 = LINE ( 'NONE', #2119, #1260 ) ;
#3426 = EDGE_CURVE ( 'NONE', #5543, #4390, #3665, .T. ) ;
#3427 = CARTESIAN_POINT ( 'NONE',  ( 245.0000000000000000, -8.660254037844389075, 140.0000000000000000 ) ) ;
#3428 = VERTEX_POINT ( 'NONE', #6452 ) ;
#3429 = LINE ( 'NONE', #529, #2990 ) ;
#3430 = LINE ( 'NONE', #6752, #305 ) ;
#3431 = DIRECTION ( 'NONE',  ( 1.000000000000000000, 0.000000000000000000, 0.000000000000000000 ) ) ;
#3432 = EDGE_CURVE ( 'NONE', #266, #4461, #274, .T. ) ;
#3433 = EDGE_LOOP ( 'NONE', ( #6863, #95, #2831, #1990 ) ) ;
#3434 = DIRECTION ( 'NONE',  ( 1.000000000000000000, 0.000000000000000000, 0.000000000000000000 ) ) ;
#3435 = ORIENTED_EDGE ( 'NONE', *, *, #5476, .T. ) ;
#3436 = EDGE_LOOP ( 'NONE', ( #2782, #2303, #7011, #6195, #1320 ) ) ;
#3437 = DIRECTION ( 'NONE',  ( 0.000000000000000000, 0.000000000000000000, 1.000000000000000000 ) ) ;
#3438 = DIRECTION ( 'NONE',  ( -1.000000000000000000, 0.000000000000000000, 0.000000000000000000 ) ) ;
#3439 = PLANE ( 'NONE',  #1329 ) ;
#3440 = CARTESIAN_POINT ( 'NONE',  ( 245.0000000000000000, 8.660254037844390851, 139.9990000000000236 ) ) ;
#3441 =( REPRESENTATION_RELATIONSHIP ('NONE','NONE', #5587, #1193 ) REPRESENTATION_RELATIONSHIP_WITH_TRANSFORMATION ( #1922 )SHAPE_REPRESENTATION_RELATIONSHIP( ) );
#3442 = ORIENTED_EDGE ( 'NONE', *, *, #4112, .T. ) ;
#3443 = DIRECTION ( 'NONE',  ( -0.000000000000000000, -0.000000000000000000, -1.000000000000000000 ) ) ;
#3444 = EDGE_LOOP ( 'NONE', ( #1300, #6344, #1541, #6899 ) ) ;
#3445 = FACE_BOUND ( 'NONE', #2476, .T. ) ;
#3446 = DIRECTION ( 'NONE',  ( 0.000000000000000000, 0.000000000000000000, 1.000000000000000000 ) ) ;
#3447 = CARTESIAN_POINT ( 'NONE',  ( 0.000000000000000000, 0.000000000000000000, 4.000000000000000000 ) ) ;
#3448 = DIRECTION ( 'NONE',  ( 1.000000000000000000, 0.000000000000000000, 0.000000000000000000 ) ) ;
#3449 = SURFACE_STYLE_USAGE ( .BOTH. , #6242 ) ;
#3450 = ORIENTED_EDGE ( 'NONE', *, *, #13, .F. ) ;
#3451 = EDGE_CURVE ( 'NONE', #3234, #5460, #3731, .T. ) ;
#3452 = DIRECTION ( 'NONE',  ( 0.000000000000000000, 0.000000000000000000, 1.000000000000000000 ) ) ;
#3453 = ORIENTED_EDGE ( 'NONE', *, *, #6923, .T. ) ;
#3454 = SURFACE_STYLE_FILL_AREA ( #3561 ) ;
#3455 = DIRECTION ( 'NONE',  ( -0.000000000000000000, -0.000000000000000000, 1.000000000000000000 ) ) ;
#3456 = CIRCLE ( 'NONE', #248, 2.500000000000000888 ) ;
#3457 = EDGE_LOOP ( 'NONE', ( #795, #4640, #1761, #5189 ) ) ;
#3458 = EDGE_CURVE ( 'NONE', #4157, #1780, #7202, .T. ) ;
#3459 = DIRECTION ( 'NONE',  ( 0.000000000000000000, 0.000000000000000000, 1.000000000000000000 ) ) ;
#3460 = CARTESIAN_POINT ( 'NONE',  ( 84.99999999999998579, 8.660254037844390851, 139.9990000000000236 ) ) ;
#3461 = VERTEX_POINT ( 'NONE', #5968 ) ;
#3462 = PRODUCT_DEFINITION_SHAPE ( 'NONE', 'NONE',  #7383 ) ;
#3463 = CARTESIAN_POINT ( 'NONE',  ( -4.198928548860774157, 0.8158838809860065044, -3.526471437616918170 ) ) ;
#3464 = AXIS2_PLACEMENT_3D ( 'NONE', #3255, #4437, #1592 ) ;
#3465 = VECTOR ( 'NONE', #6057, 1000.000000000000000 ) ;
#3466 = VERTEX_POINT ( 'NONE', #5887 ) ;
#3467 = ADVANCED_FACE ( 'NONE', ( #3087, #830 ), #167, .T. ) ;
#3468 = LINE ( 'NONE', #194, #155 ) ;
#3469 = DIRECTION ( 'NONE',  ( 0.000000000000000000, 0.000000000000000000, 1.000000000000000000 ) ) ;
#3470 = CARTESIAN_POINT ( 'NONE',  ( 75.00000000000001421, 8.660254037844390851, 140.0000000000000000 ) ) ;
#3471 = PLANE ( 'NONE',  #4280 ) ;
#3472 = ORIENTED_EDGE ( 'NONE', *, *, #2272, .T. ) ;
#3473 = EDGE_CURVE ( 'NONE', #6812, #2892, #2532, .T. ) ;
#3474 = FACE_OUTER_BOUND ( 'NONE', #2927, .T. ) ;
#3475 = ORIENTED_EDGE ( 'NONE', *, *, #6441, .F. ) ;
#3476 = CARTESIAN_POINT ( 'NONE',  ( 2.500000000000000000, -1.178949249685213863, 2.042000000000002924 ) ) ;
#3477 = DIRECTION ( 'NONE',  ( 0.000000000000000000, 0.000000000000000000, 1.000000000000000000 ) ) ;
#3478 = CARTESIAN_POINT ( 'NONE',  ( 4.101954839143059139, -2.368264730582948285, -3.681130640444269631 ) ) ;
#3479 = DIRECTION ( 'NONE',  ( -0.000000000000000000, 1.000000000000000000, -0.000000000000000000 ) ) ;
#3480 = VECTOR ( 'NONE', #4645, 1000.000000000000000 ) ;
#3481 = CIRCLE ( 'NONE', #4454, 2.649999999999985700 ) ;
#3482 = ADVANCED_FACE ( 'NONE', ( #4233 ), #1282, .F. ) ;
#3483 = VECTOR ( 'NONE', #1759, 1000.000000000000000 ) ;
#3484 = VERTEX_POINT ( 'NONE', #3016 ) ;
#3485 = PRODUCT_CONTEXT ( 'NONE', #3717, 'mechanical' ) ;
#3486 = LINE ( 'NONE', #2361, #1939 ) ;
#3487 = ORIENTED_EDGE ( 'NONE', *, *, #368, .T. ) ;
#3488 = CIRCLE ( 'NONE', #4466, 13.29999999999999893 ) ;
#3489 = LINE ( 'NONE', #3563, #573 ) ;
#3490 = ORIENTED_EDGE ( 'NONE', *, *, #484, .T. ) ;
#3491 = PLANE ( 'NONE',  #6961 ) ;
#3492 = AXIS2_PLACEMENT_3D ( 'NONE', #5371, #3767, #7176 ) ;
#3493 = DIRECTION ( 'NONE',  ( 1.000000000000000000, 0.000000000000000000, 0.000000000000000000 ) ) ;
#3494 = AXIS2_PLACEMENT_3D ( 'NONE', #4835, #868, #5892 ) ;
#3495 = TOROIDAL_SURFACE ( 'NONE', #6295, 11.75000000000000000, 1.050000000000000266 ) ;
#3496 = EDGE_CURVE ( 'NONE', #6812, #5946, #632, .T. ) ;
#3497 = VERTEX_POINT ( 'NONE', #6565 ) ;
#3498 = DIRECTION ( 'NONE',  ( 0.000000000000000000, 0.000000000000000000, -1.000000000000000000 ) ) ;
#3499 = EDGE_CURVE ( 'NONE', #5950, #3638, #3190, .T. ) ;
#3500 = VECTOR ( 'NONE', #1980, 1000.000000000000000 ) ;
#3501 = EDGE_LOOP ( 'NONE', ( #5742, #2692, #7036, #6067 ) ) ;
#3502 = CARTESIAN_POINT ( 'NONE',  ( 11.00000000000000000, 1.347111479062088405E-15, -121.0000000000000000 ) ) ;
#3503 = LINE ( 'NONE', #50, #4981 ) ;
#3504 = ITEM_DEFINED_TRANSFORMATION ( 'NONE', 'NONE', #1712,  #1963 ) ;
#3505 = DIRECTION ( 'NONE',  ( -0.000000000000000000, 1.000000000000000000, -0.000000000000000000 ) ) ;
#3506 = LINE ( 'NONE', #3046, #3634 ) ;
#3507 = VECTOR ( 'NONE', #5491, 1000.000000000000000 ) ;
#3508 = FILL_AREA_STYLE ('',( #6413 ) ) ;
#3509 = VERTEX_POINT ( 'NONE', #2464 ) ;
#3510 = DIRECTION ( 'NONE',  ( 1.000000000000000000, 0.000000000000000000, -0.000000000000000000 ) ) ;
#3511 = EDGE_CURVE ( 'NONE', #847, #7294, #3598, .T. ) ;
#3512 = ORIENTED_EDGE ( 'NONE', *, *, #3186, .F. ) ;
#3513 =( BOUNDED_SURFACE ( )  B_SPLINE_SURFACE ( 3, 2, ( 
 ( #1302, #5809, #7040 ),
 ( #5378, #4717, #122 ),
 ( #4677, #6371, #7009 ),
 ( #4076, #4181, #4222 ),
 ( #1234, #1380, #2376 ),
 ( #3573, #6410, #3617 ) ),
 .UNSPECIFIED., .F., .F., .T. ) 
 B_SPLINE_SURFACE_WITH_KNOTS ( ( 4, 2, 4 ),
 ( 3, 3 ),
 ( 0.02032853247518126918, 0.02278863295364821906, 0.02524873343211517240 ),
 ( 0.000000000000000000, 1.000000000000000000 ),
 .UNSPECIFIED. ) 
 GEOMETRIC_REPRESENTATION_ITEM ( )  RATIONAL_B_SPLINE_SURFACE ( (
 ( 1.000000000000000000, 0.8047781615896837382, 1.000000000000000000),
 ( 1.000000000000000000, 0.8123767586289252218, 1.000000000000000000),
 ( 1.000000000000000000, 0.8190662415564388121, 1.000000000000000000),
 ( 1.000000000000000000, 0.8192361015669026303, 1.000000000000000000),
 ( 1.000000000000000000, 0.8126135807103900266, 1.000000000000000000),
 ( 1.000000000000000000, 0.8047712338318593339, 1.000000000000000000) ) ) 
 REPRESENTATION_ITEM ( '' )  SURFACE ( )  );
#3514 = VECTOR ( 'NONE', #4604, 1000.000000000000000 ) ;
#3515 = DIRECTION ( 'NONE',  ( -0.000000000000000000, 0.000000000000000000, -1.000000000000000000 ) ) ;
#3516 = CARTESIAN_POINT ( 'NONE',  ( 386.6666666666666288, -20.00000000000000000, 162.5000000000000853 ) ) ;
#3517 = LINE ( 'NONE', #6808, #6122 ) ;
#3518 = DIRECTION ( 'NONE',  ( 1.000000000000000000, 0.000000000000000000, 0.000000000000000000 ) ) ;
#3519 = AXIS2_PLACEMENT_3D ( 'NONE', #4, #1564, #1639 ) ;
#3520 = DIRECTION ( 'NONE',  ( 0.000000000000000000, 1.224646799147351975E-16, 1.000000000000000000 ) ) ;
#3521 = EDGE_CURVE ( 'NONE', #5898, #3857, #2988, .T. ) ;
#3522 = AXIS2_PLACEMENT_3D ( 'NONE', #808, #403, #1438 ) ;
#3523 = ORIENTED_EDGE ( 'NONE', *, *, #6537, .T. ) ;
#3524 = CARTESIAN_POINT ( 'NONE',  ( 445.0000000000000000, 8.660254037844390851, 139.9990000000000236 ) ) ;
#3525 = EDGE_LOOP ( 'NONE', ( #417, #2529, #163, #5602 ) ) ;
#3526 = AXIS2_PLACEMENT_3D ( 'NONE', #4013, #5140, #5841 ) ;
#3527 =( GEOMETRIC_REPRESENTATION_CONTEXT ( 3 ) GLOBAL_UNCERTAINTY_ASSIGNED_CONTEXT ( ( #2080 ) ) GLOBAL_UNIT_ASSIGNED_CONTEXT ( ( #4291, #3769, #4853 ) ) REPRESENTATION_CONTEXT ( 'NONE', 'WORKASPACE' ) );
#3528 = ORIENTED_EDGE ( 'NONE', *, *, #2289, .F. ) ;
#3529 =( REPRESENTATION_RELATIONSHIP ('NONE','NONE', #5587, #5023 ) REPRESENTATION_RELATIONSHIP_WITH_TRANSFORMATION ( #2900 )SHAPE_REPRESENTATION_RELATIONSHIP( ) );
#3530 =( LENGTH_UNIT ( ) NAMED_UNIT ( * ) SI_UNIT ( .MILLI., .METRE. ) );
#3531 = DIRECTION ( 'NONE',  ( 0.000000000000000000, 0.000000000000000000, 1.000000000000000000 ) ) ;
#3532 = DIRECTION ( 'NONE',  ( 0.000000000000000000, -0.5000000000000012212, -0.8660254037844380415 ) ) ;
#3533 = FILL_AREA_STYLE ('',( #4107 ) ) ;
#3534 = CIRCLE ( 'NONE', #459, 2.649999999999985700 ) ;
#3535 = VERTEX_POINT ( 'NONE', #801 ) ;
#3536 = EDGE_CURVE ( 'NONE', #1502, #7340, #5357, .T. ) ;
#3537 = CARTESIAN_POINT ( 'NONE',  ( -31.74999999999995737, 0.000000000000000000, 0.000000000000000000 ) ) ;
#3538 = CARTESIAN_POINT ( 'NONE',  ( 53.33333333333330017, -20.00000000000000000, 159.8500000000001080 ) ) ;
#3539 = ITEM_DEFINED_TRANSFORMATION ( 'NONE', 'NONE', #756,  #1963 ) ;
#3540 = LINE ( 'NONE', #5919, #2879 ) ;
#3541 = CARTESIAN_POINT ( 'NONE',  ( -30.00000000000002842, -15.00000000000000000, 145.0000000000000284 ) ) ;
#3542 = ORIENTED_EDGE ( 'NONE', *, *, #24, .T. ) ;
#3543 = CARTESIAN_POINT ( 'NONE',  ( 136.6666666666666288, -14.99999999999999822, 162.5000000000000853 ) ) ;
#3544 = PRODUCT ( 'base plate', 'base plate', '', ( #3959 ) ) ;
#3545 = ORIENTED_EDGE ( 'NONE', *, *, #5847, .T. ) ;
#3546 = ORIENTED_EDGE ( 'NONE', *, *, #735, .T. ) ;
#3547 = CARTESIAN_POINT ( 'NONE',  ( 155.0000000000000000, 8.660254037844390851, 139.9990000000000236 ) ) ;
#3548 = CARTESIAN_POINT ( 'NONE',  ( 0.000000000000000000, 0.000000000000000000, 121.0000000000000000 ) ) ;
#3549 = DIRECTION ( 'NONE',  ( 0.000000000000000000, 1.000000000000000000, 0.000000000000000000 ) ) ;
#3550 = CARTESIAN_POINT ( 'NONE',  ( 1.567478505476134606E-15, 4.618802153517012066, -5.000000000000000000 ) ) ;
#3551 = EDGE_CURVE ( 'NONE', #598, #468, #5032, .T. ) ;
#3552 = CARTESIAN_POINT ( 'NONE',  ( 219.9999999999999716, -20.00000000000000000, -159.8500000000001080 ) ) ;
#3553 = EDGE_CURVE ( 'NONE', #2018, #1972, #4908, .T. ) ;
#3554 = CARTESIAN_POINT ( 'NONE',  ( 303.3333333333333144, -25.00000000000000000, 159.8500000000001080 ) ) ;
#3555 = ORIENTED_EDGE ( 'NONE', *, *, #2701, .F. ) ;
#3556 = ORIENTED_EDGE ( 'NONE', *, *, #511, .T. ) ;
#3557 = ITEM_DEFINED_TRANSFORMATION ( 'NONE', 'NONE', #6024,  #1963 ) ;
#3558 = CARTESIAN_POINT ( 'NONE',  ( -30.00000000000002842, 15.00000000000000000, 140.0000000000000000 ) ) ;
#3559 = ORIENTED_EDGE ( 'NONE', *, *, #4340, .F. ) ;
#3560 = EDGE_CURVE ( 'NONE', #4557, #5461, #1030, .T. ) ;
#3561 = FILL_AREA_STYLE ('',( #37 ) ) ;
#3562 = EDGE_CURVE ( 'NONE', #432, #271, #5464, .T. ) ;
#3563 = CARTESIAN_POINT ( 'NONE',  ( 84.99999999999998579, -8.660254037844389075, 139.9990000000000236 ) ) ;
#3564 = ORIENTED_EDGE ( 'NONE', *, *, #3222, .T. ) ;
#3565 = DIRECTION ( 'NONE',  ( 0.000000000000000000, 0.000000000000000000, -1.000000000000000000 ) ) ;
#3566 = FACE_OUTER_BOUND ( 'NONE', #6734, .T. ) ;
#3567 =( NAMED_UNIT ( * ) PLANE_ANGLE_UNIT ( ) SI_UNIT ( $, .RADIAN. ) );
#3568 = EDGE_LOOP ( 'NONE', ( #1927, #2799 ) ) ;
#3569 = EDGE_CURVE ( 'NONE', #6701, #2565, #1335, .T. ) ;
#3570 = TOROIDAL_SURFACE ( 'NONE', #3211, 4.000000000000000000, 0.2500000000000000000 ) ;
#3571 = DIRECTION ( 'NONE',  ( -1.000000000000000000, 0.000000000000000000, 0.000000000000000000 ) ) ;
#3572 = CONTEXT_DEPENDENT_SHAPE_REPRESENTATION ( #4827, #1266 ) ;
#3573 = CARTESIAN_POINT ( 'NONE',  ( 4.175648173966055587, -2.207990556236547608, -3.469390959564065291 ) ) ;
#3574 = CARTESIAN_POINT ( 'NONE',  ( -13.50000000000000000, 1.653273178848926867E-15, 121.0000000000000000 ) ) ;
#3575 = SURFACE_SIDE_STYLE ('',( #3619 ) ) ;
#3576 = ORIENTED_EDGE ( 'NONE', *, *, #361, .F. ) ;
#3577 = FACE_OUTER_BOUND ( 'NONE', #1295, .T. ) ;
#3578 = EDGE_CURVE ( 'NONE', #7308, #3535, #2697, .T. ) ;
#3579 = AXIS2_PLACEMENT_3D ( 'NONE', #512, #5178, #1180 ) ;
#3580 = AXIS2_PLACEMENT_3D ( 'NONE', #4403, #2019, #2665 ) ;
#3581 = ORIENTED_EDGE ( 'NONE', *, *, #768, .F. ) ;
#3582 = PRODUCT_DEFINITION_SHAPE ( 'NONE', 'NONE',  #7375 ) ;
#3583 = ORIENTED_EDGE ( 'NONE', *, *, #6062, .T. ) ;
#3584 = CARTESIAN_POINT ( 'NONE',  ( 11.00000000000000000, 1.347111479062088405E-15, 125.0000000000000000 ) ) ;
#3585 = CARTESIAN_POINT ( 'NONE',  ( -0.6810597143197697489, -4.461075778259609770, -3.598441714920717516 ) ) ;
#3586 = DIRECTION ( 'NONE',  ( 1.000000000000000000, 0.000000000000000000, 0.000000000000000000 ) ) ;
#3587 = LINE ( 'NONE', #5248, #427 ) ;
#3588 = DIRECTION ( 'NONE',  ( 0.000000000000000000, -0.000000000000000000, 1.000000000000000000 ) ) ;
#3589 = EDGE_CURVE ( 'NONE', #5499, #4862, #7196, .T. ) ;
#3590 = CARTESIAN_POINT ( 'NONE',  ( -1.240299975428113101E-15, -4.647091401871173311, -3.572172305156514849 ) ) ;
#3591 = EDGE_CURVE ( 'NONE', #807, #7221, #6759, .T. ) ;
#3592 = EDGE_LOOP ( 'NONE', ( #5804, #869 ) ) ;
#3593 = EDGE_LOOP ( 'NONE', ( #4725, #5527, #2596, #925 ) ) ;
#3594 = AXIS2_PLACEMENT_3D ( 'NONE', #5275, #4752, #2484 ) ;
#3595 = CONTEXT_DEPENDENT_SHAPE_REPRESENTATION ( #6909, #1468 ) ;
#3596 = FACE_OUTER_BOUND ( 'NONE', #60, .T. ) ;
#3597 = ORIENTED_EDGE ( 'NONE', *, *, #926, .T. ) ;
#3598 = CIRCLE ( 'NONE', #6740, 2.649999999999985700 ) ;
#3599 = CARTESIAN_POINT ( 'NONE',  ( 0.000000000000000000, 0.000000000000000000, -200.0000000000000000 ) ) ;
#3600 = UNCERTAINTY_MEASURE_WITH_UNIT (LENGTH_MEASURE( 1.000000000000000082E-05 ), #4741, 'distance_accuracy_value', 'NONE');
#3601 = EDGE_CURVE ( 'NONE', #6365, #1344, #6855, .T. ) ;
#3602 = VERTEX_POINT ( 'NONE', #1545 ) ;
#3603 = ORIENTED_EDGE ( 'NONE', *, *, #1864, .F. ) ;
#3604 = PRODUCT ( 'socket head cap screw_iso_ISO 4762 M5 x 20 - 20N', 'socket head cap screw_iso_ISO 4762 M5 x 20 - 20N', '', ( #1744 ) ) ;
#3605 = CARTESIAN_POINT ( 'NONE',  ( -1.799999999999996048, 0.000000000000000000, 0.000000000000000000 ) ) ;
#3606 = AXIS2_PLACEMENT_3D ( 'NONE', #7207, #6695, #362 ) ;
#3607 = ORIENTED_EDGE ( 'NONE', *, *, #7038, .F. ) ;
#3608 = CARTESIAN_POINT ( 'NONE',  ( 114.9999999999999858, -8.660254037844389075, 140.0000000000000000 ) ) ;
#3609 = EDGE_CURVE ( 'NONE', #586, #4318, #6491, .T. ) ;
#3610 = ORIENTED_EDGE ( 'NONE', *, *, #7060, .T. ) ;
#3611 = CIRCLE ( 'NONE', #6268, 0.2000000000000022593 ) ;
#3612 = AXIS2_PLACEMENT_3D ( 'NONE', #5492, #4989, #4420 ) ;
#3613 = TOROIDAL_SURFACE ( 'NONE', #6154, 5.384454397937118664, 0.5155456020628804703 ) ;
#3614 = VECTOR ( 'NONE', #2017, 1000.000000000000000 ) ;
#3615 = CLOSED_SHELL ( 'NONE', ( #915, #788, #2085, #1558, #5890, #1733, #2237, #244, #3987, #3798, #4726, #3368, #5130, #4033, #6274, #4489, #6732, #5730, #2130, #7232, #4170, #1626, #4374, #4889, #1941, #3269, #6428, #5261, #1899, #3678, #2750, #3091, #7263, #4781, #6289, #1287, #2192, #5343, #6631, #3082, #1779, #3136, #7093, #2549, #3924, #4959, #2584, #3901, #5918, #6713, #4045, #4635, #1404, #1988, #4702, #2987, #4661, #223, #826, #1107, #1191, #6478, #4293, #3357, #4473, #276 ) ) ;
#3616 = DIRECTION ( 'NONE',  ( 1.000000000000000000, 0.000000000000000000, 0.000000000000000000 ) ) ;
#3617 = CARTESIAN_POINT ( 'NONE',  ( 4.236525694536557474, -2.416953475386482530, -3.751298745799839462 ) ) ;
#3618 = CARTESIAN_POINT ( 'NONE',  ( -6.259644161404860030E-16, -4.618802153517027165, -5.000000000000000000 ) ) ;
#3619 = SURFACE_STYLE_FILL_AREA ( #3508 ) ;
#3620 = APPLICATION_CONTEXT ( 'automotive_design' ) ;
#3621 = EDGE_LOOP ( 'NONE', ( #1533, #4079 ) ) ;
#3622 = CARTESIAN_POINT ( 'NONE',  ( 355.0000000000000000, 8.660254037844390851, 145.0000000000000284 ) ) ;
#3623 = AXIS2_PLACEMENT_3D ( 'NONE', #6343, #1729, #3331 ) ;
#3624 = ORIENTED_EDGE ( 'NONE', *, *, #3790, .F. ) ;
#3625 = EDGE_LOOP ( 'NONE', ( #325, #595, #4094, #5341 ) ) ;
#3626 = LINE ( 'NONE', #165, #1323 ) ;
#3627 = CARTESIAN_POINT ( 'NONE',  ( 4.000000000000000000, 0.000000000000000000, 0.000000000000000000 ) ) ;
#3628 = CIRCLE ( 'NONE', #3259, 2.649999999999985700 ) ;
#3629 = PRESENTATION_LAYER_ASSIGNMENT (  '', '', ( #5917 ) ) ;
#3630 = CARTESIAN_POINT ( 'NONE',  ( -4.000000000000000000, -1.942223658245633811, -0.3516579909967644246 ) ) ;
#3631 = CARTESIAN_POINT ( 'NONE',  ( 5.200000000000002842, 0.000000000000000000, 0.000000000000000000 ) ) ;
#3632 = CARTESIAN_POINT ( 'NONE',  ( -2.000000000000007550, -3.464101615137749945, 0.000000000000000000 ) ) ;
#3633 = DIRECTION ( 'NONE',  ( 0.000000000000000000, 1.000000000000000000, 0.000000000000000000 ) ) ;
#3634 = VECTOR ( 'NONE', #1274, 1000.000000000000000 ) ;
#3635 = AXIS2_PLACEMENT_3D ( 'NONE', #5973, #6498, #836 ) ;
#3636 = ORIENTED_EDGE ( 'NONE', *, *, #6184, .T. ) ;
#3637 = CARTESIAN_POINT ( 'NONE',  ( 219.9999999999999716, -25.00000000000000000, -159.8500000000001080 ) ) ;
#3638 = VERTEX_POINT ( 'NONE', #4998 ) ;
#3639 = EDGE_CURVE ( 'NONE', #6561, #1168, #6718, .T. ) ;
#3640 = AXIS2_PLACEMENT_3D ( 'NONE', #6147, #3493, #7032 ) ;
#3641 = AXIS2_PLACEMENT_3D ( 'NONE', #3548, #129, #6318 ) ;
#3642 = PLANE ( 'NONE',  #782 ) ;
#3643 = ORIENTED_EDGE ( 'NONE', *, *, #193, .T. ) ;
#3644 = VECTOR ( 'NONE', #2765, 1000.000000000000000 ) ;
#3645 = ORIENTED_EDGE ( 'NONE', *, *, #3072, .T. ) ;
#3646 = DIRECTION ( 'NONE',  ( -0.000000000000000000, 0.000000000000000000, 1.000000000000000000 ) ) ;
#3647 = DIRECTION ( 'NONE',  ( 0.000000000000000000, -0.000000000000000000, 1.000000000000000000 ) ) ;
#3648 = EDGE_CURVE ( 'NONE', #4530, #1288, #396, .T. ) ;
#3649 = ADVANCED_FACE ( 'NONE', ( #3700 ), #352, .T. ) ;
#3650 = AXIS2_PLACEMENT_3D ( 'NONE', #4177, #6364, #83 ) ;
#3651 = ORIENTED_EDGE ( 'NONE', *, *, #6241, .F. ) ;
#3652 = PRODUCT_DEFINITION_SHAPE ( 'NONE', 'NONE',  #7402 ) ;
#3653 = DIRECTION ( 'NONE',  ( -1.000000000000000000, -0.000000000000000000, -0.000000000000000000 ) ) ;
#3654 = EDGE_LOOP ( 'NONE', ( #1227, #236, #1822, #2849 ) ) ;
#3655 = LINE ( 'NONE', #5454, #6981 ) ;
#3656 = FACE_OUTER_BOUND ( 'NONE', #6134, .T. ) ;
#3657 = DIRECTION ( 'NONE',  ( -0.000000000000000000, 1.000000000000000000, -0.000000000000000000 ) ) ;
#3658 = EDGE_CURVE ( 'NONE', #5826, #7027, #985, .T. ) ;
#3659 = ORIENTED_EDGE ( 'NONE', *, *, #2403, .T. ) ;
#3660 = DIRECTION ( 'NONE',  ( 1.000000000000000000, 0.000000000000000000, 0.000000000000000000 ) ) ;
#3661 = VERTEX_POINT ( 'NONE', #4394 ) ;
#3662 = EDGE_LOOP ( 'NONE', ( #2380, #6117, #900, #3285 ) ) ;
#3663 = FACE_OUTER_BOUND ( 'NONE', #5937, .T. ) ;
#3664 = CARTESIAN_POINT ( 'NONE',  ( 4.000000000000000000, 0.7924765000094659007, -0.05906175389889852662 ) ) ;
#3665 = LINE ( 'NONE', #7019, #872 ) ;
#3666 = PLANE ( 'NONE',  #3130 ) ;
#3667 = CARTESIAN_POINT ( 'NONE',  ( -30.00000000000002842, -20.00000000000000000, 180.0000000000000284 ) ) ;
#3668 = DIRECTION ( 'NONE',  ( -0.000000000000000000, -0.000000000000000000, 1.000000000000000000 ) ) ;
#3669 = EDGE_LOOP ( 'NONE', ( #3475, #1874, #5685, #2922 ) ) ;
#3670 = PRODUCT_DEFINITION_SHAPE ( 'NONE', 'NONE',  #7346 ) ;
#3671 = ITEM_DEFINED_TRANSFORMATION ( 'NONE', 'NONE', #5297,  #1963 ) ;
#3672 = DIRECTION ( 'NONE',  ( 0.000000000000000000, 0.000000000000000000, -1.000000000000000000 ) ) ;
#3673 = VERTEX_POINT ( 'NONE', #7158 ) ;
#3674 = DIRECTION ( 'NONE',  ( 1.000000000000000000, 0.000000000000000000, 0.000000000000000000 ) ) ;
#3675 = FILL_AREA_STYLE_COLOUR ( '', #662 ) ;
#3676 =( REPRESENTATION_RELATIONSHIP ('NONE','NONE', #5587, #5023 ) REPRESENTATION_RELATIONSHIP_WITH_TRANSFORMATION ( #4737 )SHAPE_REPRESENTATION_RELATIONSHIP( ) );
#3677 = CARTESIAN_POINT ( 'NONE',  ( -13.50000000000000000, 1.653273178848926867E-15, 121.0000000000000000 ) ) ;
#3678 = ADVANCED_FACE ( 'NONE', ( #2168 ), #472, .F. ) ;
#3679 = ORIENTED_EDGE ( 'NONE', *, *, #2225, .F. ) ;
#3680 = ORIENTED_EDGE ( 'NONE', *, *, #511, .F. ) ;
#3681 = DIRECTION ( 'NONE',  ( -1.000000000000000000, -0.000000000000000000, -0.000000000000000000 ) ) ;
#3682 = CARTESIAN_POINT ( 'NONE',  ( -4.024497503033519941, -2.323544716729390558, -3.572167766733381544 ) ) ;
#3683 = DIRECTION ( 'NONE',  ( -0.000000000000000000, -0.000000000000000000, 1.000000000000000000 ) ) ;
#3684 = LINE ( 'NONE', #2121, #6539 ) ;
#3685 = EDGE_LOOP ( 'NONE', ( #2588, #1095, #5352, #5986 ) ) ;
#3686 = EDGE_CURVE ( 'NONE', #1987, #763, #2519, .T. ) ;
#3687 = LINE ( 'NONE', #6630, #6255 ) ;
#3688 = ITEM_DEFINED_TRANSFORMATION ( 'NONE', 'NONE', #6153,  #1963 ) ;
#3689 = CARTESIAN_POINT ( 'NONE',  ( 355.0000000000000000, -8.660254037844389075, 139.9990000000000236 ) ) ;
#3690 = FACE_BOUND ( 'NONE', #4982, .T. ) ;
#3691 = CARTESIAN_POINT ( 'NONE',  ( 40.00000000000000000, 0.000000000000000000, -123.0000000000000000 ) ) ;
#3692 = ORIENTED_EDGE ( 'NONE', *, *, #3451, .F. ) ;
#3693 = CARTESIAN_POINT ( 'NONE',  ( -3.511755186886750479, 2.826662030176366081, -3.597382984111578086 ) ) ;
#3694 = CIRCLE ( 'NONE', #1673, 13.50000000000000000 ) ;
#3695 = EDGE_CURVE ( 'NONE', #2671, #3602, #1460, .T. ) ;
#3696 = VERTEX_POINT ( 'NONE', #5737 ) ;
#3697 = VERTEX_POINT ( 'NONE', #5660 ) ;
#3698 = CARTESIAN_POINT ( 'NONE',  ( 470.0000000000000000, -20.00000000000000000, 200.0000000000000000 ) ) ;
#3699 = CARTESIAN_POINT ( 'NONE',  ( -2.836893136758495970, -3.208949435745868328, -3.505054077164885484 ) ) ;
#3700 = FACE_OUTER_BOUND ( 'NONE', #4683, .T. ) ;
#3701 = FACE_OUTER_BOUND ( 'NONE', #811, .T. ) ;
#3702 = EDGE_CURVE ( 'NONE', #4019, #6406, #5770, .T. ) ;
#3703 = CARTESIAN_POINT ( 'NONE',  ( 0.2500000000000002220, 0.000000000000000000, 4.250000000000000000 ) ) ;
#3704 = VERTEX_POINT ( 'NONE', #544 ) ;
#3705 = AXIS2_PLACEMENT_3D ( 'NONE', #673, #7326, #2178 ) ;
#3706 = AXIS2_PLACEMENT_3D ( 'NONE', #4867, #4347, #2530 ) ;
#3707 = CARTESIAN_POINT ( 'NONE',  ( 2.682243648011666703, 3.070208061305304881, -0.04852650426601266831 ) ) ;
#3708 = DIRECTION ( 'NONE',  ( 1.000000000000000000, 0.000000000000000000, 0.000000000000000000 ) ) ;
#3709 = VERTEX_POINT ( 'NONE', #1065 ) ;
#3710 = CARTESIAN_POINT ( 'NONE',  ( -2.345747346278108214, 3.264484291692489215, -0.01223254789873409049 ) ) ;
#3711 =( NAMED_UNIT ( * ) SI_UNIT ( $, .STERADIAN. ) SOLID_ANGLE_UNIT ( ) );
#3712 = EDGE_CURVE ( 'NONE', #1411, #5253, #4614, .T. ) ;
#3713 = LINE ( 'NONE', #6016, #2917 ) ;
#3714 = EDGE_LOOP ( 'NONE', ( #5212, #3062, #4302, #4109 ) ) ;
#3715 = DIRECTION ( 'NONE',  ( 0.000000000000000000, 0.000000000000000000, -1.000000000000000000 ) ) ;
#3716 = ORIENTED_EDGE ( 'NONE', *, *, #1800, .T. ) ;
#3717 = APPLICATION_CONTEXT ( 'automotive_design' ) ;
#3718 = CARTESIAN_POINT ( 'NONE',  ( -4.000000000000000000, -2.309401076758512694, -3.433295621305382461 ) ) ;
#3719 = AXIS2_PLACEMENT_3D ( 'NONE', #4938, #850, #5416 ) ;
#3720 = DIRECTION ( 'NONE',  ( 0.000000000000000000, 1.000000000000000000, 0.000000000000000000 ) ) ;
#3721 = LINE ( 'NONE', #6027, #1270 ) ;
#3722 = VERTEX_POINT ( 'NONE', #5111 ) ;
#3723 = CARTESIAN_POINT ( 'NONE',  ( -0.7826237921249277196, 1.353234713057825478E-15, 11.05000000000000071 ) ) ;
#3724 = ADVANCED_FACE ( 'NONE', ( #6866 ), #3406, .F. ) ;
#3725 = CARTESIAN_POINT ( 'NONE',  ( 8.673617379884035472E-16, 4.618802153517012954, 0.000000000000000000 ) ) ;
#3726 = CARTESIAN_POINT ( 'NONE',  ( 0.000000000000000000, 0.000000000000000000, -0.2800830152838844622 ) ) ;
#3727 = DIRECTION ( 'NONE',  ( -1.000000000000000000, 0.000000000000000000, 0.000000000000000000 ) ) ;
#3728 = ORIENTED_EDGE ( 'NONE', *, *, #5596, .F. ) ;
#3729 = DIRECTION ( 'NONE',  ( 1.000000000000000000, 0.000000000000000000, 0.000000000000000000 ) ) ;
#3730 = PRODUCT_DEFINITION_SHAPE ( 'NONE', 'NONE',  #7358 ) ;
#3731 = CIRCLE ( 'NONE', #530, 11.05000000000000071 ) ;
#3732 = AXIS2_PLACEMENT_3D ( 'NONE', #4457, #533, #6858 ) ;
#3733 = AXIS2_PLACEMENT_3D ( 'NONE', #4813, #2996, #7109 ) ;
#3734 = ORIENTED_EDGE ( 'NONE', *, *, #113, .T. ) ;
#3735 = PRODUCT_DEFINITION_CONTEXT ( 'detailed design', #4775, 'design' ) ;
#3736 = ORIENTED_EDGE ( 'NONE', *, *, #1571, .T. ) ;
#3737 = PLANE ( 'NONE',  #5628 ) ;
#3738 = PLANE ( 'NONE',  #1262 ) ;
#3739 = DIRECTION ( 'NONE',  ( -0.000000000000000000, -0.000000000000000000, 1.000000000000000000 ) ) ;
#3740 = CARTESIAN_POINT ( 'NONE',  ( 136.6666666666666288, -20.00000000000000000, -162.5000000000000853 ) ) ;
#3741 = VECTOR ( 'NONE', #6584, 1000.000000000000000 ) ;
#3742 = CARTESIAN_POINT ( 'NONE',  ( 2.500000000000000000, -1.178949249685213863, 2.042000000000002924 ) ) ;
#3743 = AXIS2_PLACEMENT_3D ( 'NONE', #6105, #6624, #3184 ) ;
#3744 = EDGE_CURVE ( 'NONE', #450, #6179, #1097, .T. ) ;
#3745 = CARTESIAN_POINT ( 'NONE',  ( -5.000000000000000888, 8.660254037844390851, 145.0000000000000284 ) ) ;
#3746 = CARTESIAN_POINT ( 'NONE',  ( 0.000000000000000000, 0.000000000000000000, 0.000000000000000000 ) ) ;
#3747 = CARTESIAN_POINT ( 'NONE',  ( 1.999999999999994893, 0.000000000000000000, 0.000000000000000000 ) ) ;
#3748 = EDGE_CURVE ( 'NONE', #2773, #2072, #5142, .T. ) ;
#3749 = B_SPLINE_CURVE_WITH_KNOTS ( 'NONE', 3,
 ( #125, #6447, #1383, #5211, #4755, #3008, #4226, #2458 ),
 .UNSPECIFIED., .F., .F.,
 ( 4, 2, 2, 4 ),
 ( 0.000000000000000000, 0.002450665683189818828, 0.003675998524784728459, 0.004901331366379638524 ),
 .UNSPECIFIED. ) ;
#3750 = ORIENTED_EDGE ( 'NONE', *, *, #5026, .F. ) ;
#3751 = VECTOR ( 'NONE', #6531, 1000.000000000000000 ) ;
#3752 = COLOUR_RGB ( '',0.8941176470588234615, 0.8941176470588234615, 0.8941176470588234615 ) ;
#3753 = DIRECTION ( 'NONE',  ( 1.000000000000000000, 0.000000000000000000, 0.000000000000000000 ) ) ;
#3754 = CARTESIAN_POINT ( 'NONE',  ( 114.9999999999999858, 8.660254037844390851, 139.9990000000000236 ) ) ;
#3755 = ORIENTED_EDGE ( 'NONE', *, *, #1840, .T. ) ;
#3756 = FILL_AREA_STYLE ('',( #7206 ) ) ;
#3757 = EDGE_CURVE ( 'NONE', #214, #719, #2287, .T. ) ;
#3758 = AXIS2_PLACEMENT_3D ( 'NONE', #4753, #5312, #7076 ) ;
#3759 = FACE_OUTER_BOUND ( 'NONE', #2646, .T. ) ;
#3760 = AXIS2_PLACEMENT_3D ( 'NONE', #6633, #4860, #4383 ) ;
#3761 = CARTESIAN_POINT ( 'NONE',  ( 0.000000000000000000, 0.000000000000000000, -0.3080913168122742518 ) ) ;
#3762 = ORIENTED_EDGE ( 'NONE', *, *, #1026, .T. ) ;
#3763 = CARTESIAN_POINT ( 'NONE',  ( 280.0000000000000000, 0.000000000000000000, 0.000000000000000000 ) ) ;
#3764 = VECTOR ( 'NONE', #6927, 1000.000000000000000 ) ;
#3765 = ORIENTED_EDGE ( 'NONE', *, *, #1567, .T. ) ;
#3766 = VECTOR ( 'NONE', #1552, 1000.000000000000000 ) ;
#3767 = DIRECTION ( 'NONE',  ( 0.000000000000000000, 0.000000000000000000, -1.000000000000000000 ) ) ;
#3768 = DIRECTION ( 'NONE',  ( -0.000000000000000000, 0.000000000000000000, 1.000000000000000000 ) ) ;
#3769 =( NAMED_UNIT ( * ) PLANE_ANGLE_UNIT ( ) SI_UNIT ( $, .RADIAN. ) );
#3770 = ORIENTED_EDGE ( 'NONE', *, *, #1768, .F. ) ;
#3771 = CYLINDRICAL_SURFACE ( 'NONE', #6029, 2.649999999999985700 ) ;
#3772 = FACE_OUTER_BOUND ( 'NONE', #3284, .T. ) ;
#3773 = CARTESIAN_POINT ( 'NONE',  ( 355.0000000000000000, 8.660254037844390851, 139.9990000000000236 ) ) ;
#3774 = VECTOR ( 'NONE', #2852, 1000.000000000000000 ) ;
#3775 = DIRECTION ( 'NONE',  ( 0.000000000000000000, 0.000000000000000000, 1.000000000000000000 ) ) ;
#3776 = ORIENTED_EDGE ( 'NONE', *, *, #1393, .F. ) ;
#3777 = FACE_OUTER_BOUND ( 'NONE', #6330, .T. ) ;
#3778 = EDGE_CURVE ( 'NONE', #4228, #6725, #2245, .T. ) ;
#3779 = EDGE_LOOP ( 'NONE', ( #2745, #7138 ) ) ;
#3780 = AXIS2_PLACEMENT_3D ( 'NONE', #6782, #2295, #6296 ) ;
#3781 = ORIENTED_EDGE ( 'NONE', *, *, #4101, .F. ) ;
#3782 = FACE_OUTER_BOUND ( 'NONE', #5638, .T. ) ;
#3783 = DIRECTION ( 'NONE',  ( 1.000000000000000000, 0.000000000000000000, 0.000000000000000000 ) ) ;
#3784 = CARTESIAN_POINT ( 'NONE',  ( 3.680118525130245732, -2.494084732383344605, -0.3507732604232533524 ) ) ;
#3785 = CARTESIAN_POINT ( 'NONE',  ( -4.000000000000000000, 0.9868501483902560878, -0.09357334158579519445 ) ) ;
#3786 = DIRECTION ( 'NONE',  ( 1.000000000000000000, 0.000000000000000000, 0.000000000000000000 ) ) ;
#3787 = CARTESIAN_POINT ( 'NONE',  ( 13.50000000000000000, 1.653273178848926867E-15, -121.0000000000000000 ) ) ;
#3788 = DIRECTION ( 'NONE',  ( -0.000000000000000000, -1.000000000000000000, -0.000000000000000000 ) ) ;
#3789 = ORIENTED_EDGE ( 'NONE', *, *, #2003, .F. ) ;
#3790 = EDGE_CURVE ( 'NONE', #709, #6701, #6266, .T. ) ;
#3791 = CARTESIAN_POINT ( 'NONE',  ( -11.00000000000000000, 0.000000000000000000, 125.0000000000000000 ) ) ;
#3792 = LINE ( 'NONE', #806, #3875 ) ;
#3793 = ADVANCED_FACE ( 'NONE', ( #5707 ), #4043, .F. ) ;
#3794 =( NAMED_UNIT ( * ) PLANE_ANGLE_UNIT ( ) SI_UNIT ( $, .RADIAN. ) );
#3795 = CARTESIAN_POINT ( 'NONE',  ( 1.567478505476135000E-15, 4.618802153517012954, -3.504269196027527844 ) ) ;
#3796 = DIRECTION ( 'NONE',  ( -0.000000000000000000, 1.000000000000000000, 0.000000000000000000 ) ) ;
#3797 = ORIENTED_EDGE ( 'NONE', *, *, #2104, .F. ) ;
#3798 = ADVANCED_FACE ( 'NONE', ( #1705 ), #524, .F. ) ;
#3799 = ORIENTED_EDGE ( 'NONE', *, *, #4602, .F. ) ;
#3800 = EDGE_CURVE ( 'NONE', #5197, #6342, #3227, .T. ) ;
#3801 = CARTESIAN_POINT ( 'NONE',  ( 440.0000000000000000, 0.000000000000000000, 0.000000000000000000 ) ) ;
#3802 = VERTEX_POINT ( 'NONE', #4509 ) ;
#3803 = PRODUCT_DEFINITION_SHAPE ( 'NONE', 'NONE',  #7369 ) ;
#3804 = DIRECTION ( 'NONE',  ( -1.000000000000000000, 0.000000000000000000, 0.000000000000000000 ) ) ;
#3805 = FACE_OUTER_BOUND ( 'NONE', #6262, .T. ) ;
#3806 = DIRECTION ( 'NONE',  ( 1.000000000000000000, 0.000000000000000000, 0.000000000000000000 ) ) ;
#3807 = ORIENTED_EDGE ( 'NONE', *, *, #6912, .F. ) ;
#3808 = DIRECTION ( 'NONE',  ( -1.000000000000000000, -0.000000000000000000, -0.000000000000000000 ) ) ;
#3809 = ITEM_DEFINED_TRANSFORMATION ( 'NONE', 'NONE', #56,  #1963 ) ;
#3810 = PLANE ( 'NONE',  #6960 ) ;
#3811 = FACE_OUTER_BOUND ( 'NONE', #1568, .T. ) ;
#3812 = DIRECTION ( 'NONE',  ( 0.000000000000000000, 0.000000000000000000, 1.000000000000000000 ) ) ;
#3813 = ORIENTED_EDGE ( 'NONE', *, *, #5722, .T. ) ;
#3814 = DIRECTION ( 'NONE',  ( 0.000000000000000000, 0.000000000000000000, 1.000000000000000000 ) ) ;
#3815 = EDGE_CURVE ( 'NONE', #732, #4657, #1619, .T. ) ;
#3816 = EDGE_LOOP ( 'NONE', ( #6576, #4815, #493, #4325, #3297 ) ) ;
#3817 = VERTEX_POINT ( 'NONE', #6907 ) ;
#3818 = CARTESIAN_POINT ( 'NONE',  ( 24.55500000000002103, 0.000000000000000000, 0.000000000000000000 ) ) ;
#3819 = DIRECTION ( 'NONE',  ( 1.000000000000000000, 0.000000000000000000, 0.000000000000000000 ) ) ;
#3820 = CONTEXT_DEPENDENT_SHAPE_REPRESENTATION ( #1537, #2659 ) ;
#3821 = CARTESIAN_POINT ( 'NONE',  ( 1.800000000000001155, 0.000000000000000000, -13.29999999999999893 ) ) ;
#3822 = CARTESIAN_POINT ( 'NONE',  ( -5.000000000000000888, 0.000000000000000000, -140.0000000000000000 ) ) ;
#3823 = CARTESIAN_POINT ( 'NONE',  ( 5.000000000000004441, 0.000000000000000000, 0.000000000000000000 ) ) ;
#3824 = DIRECTION ( 'NONE',  ( 1.000000000000000000, 0.000000000000000000, 0.000000000000000000 ) ) ;
#3825 =( REPRESENTATION_RELATIONSHIP ('NONE','NONE', #5587, #951 ) REPRESENTATION_RELATIONSHIP_WITH_TRANSFORMATION ( #5706 )SHAPE_REPRESENTATION_RELATIONSHIP( ) );
#3826 = VERTEX_POINT ( 'NONE', #4574 ) ;
#3827 = DIRECTION ( 'NONE',  ( -0.000000000000000000, 1.000000000000000000, -0.000000000000000000 ) ) ;
#3828 = FACE_OUTER_BOUND ( 'NONE', #5974, .T. ) ;
#3829 = DIRECTION ( 'NONE',  ( -0.000000000000000000, -0.000000000000000000, 1.000000000000000000 ) ) ;
#3830 =( LENGTH_UNIT ( ) NAMED_UNIT ( * ) SI_UNIT ( .MILLI., .METRE. ) );
#3831 = AXIS2_PLACEMENT_3D ( 'NONE', #470, #5703, #1068 ) ;
#3832 = EDGE_CURVE ( 'NONE', #4934, #3899, #1602, .T. ) ;
#3833 = LINE ( 'NONE', #7169, #6497 ) ;
#3834 = ADVANCED_FACE ( 'NONE', ( #1204 ), #3439, .F. ) ;
#3835 = DIRECTION ( 'NONE',  ( -0.000000000000000000, 1.000000000000000000, -0.000000000000000000 ) ) ;
#3836 = AXIS2_PLACEMENT_3D ( 'NONE', #28, #222, #2252 ) ;
#3837 = EDGE_LOOP ( 'NONE', ( #3196, #5860, #2938, #4723 ) ) ;
#3838 = EDGE_LOOP ( 'NONE', ( #7210, #1, #5824, #1188 ) ) ;
#3839 = B_SPLINE_CURVE_WITH_KNOTS ( 'NONE', 3,
 ( #4405, #1477, #1042, #4921, #3795, #4438 ),
 .UNSPECIFIED., .F., .F.,
 ( 4, 2, 4 ),
 ( -3.640115492407174633E-06, 0.0002066546034006553863, 0.0004169493222937179812 ),
 .UNSPECIFIED. ) ;
#3840 = CARTESIAN_POINT ( 'NONE',  ( 280.0000000000000000, 0.000000000000000000, 0.000000000000000000 ) ) ;
#3841 = ORIENTED_EDGE ( 'NONE', *, *, #2416, .T. ) ;
#3842 = CARTESIAN_POINT ( 'NONE',  ( -30.00000000000002842, -15.00000000000000000, 140.0000000000000000 ) ) ;
#3843 = EDGE_CURVE ( 'NONE', #4557, #4971, #2312, .T. ) ;
#3844 = DIRECTION ( 'NONE',  ( 0.000000000000000000, 0.000000000000000000, -1.000000000000000000 ) ) ;
#3845 = CARTESIAN_POINT ( 'NONE',  ( -4.211140560182196957, -2.431303136016552013, -3.745885042887436178 ) ) ;
#3846 = ORIENTED_EDGE ( 'NONE', *, *, #4163, .F. ) ;
#3847 = AXIS2_PLACEMENT_3D ( 'NONE', #3725, #7225, #6552 ) ;
#3848 = CARTESIAN_POINT ( 'NONE',  ( -2.100000000000000089, 2.571758278209441957E-16, -0.2800830152838844622 ) ) ;
#3849 = ITEM_DEFINED_TRANSFORMATION ( 'NONE', 'NONE', #2419,  #1963 ) ;
#3850 = FACE_OUTER_BOUND ( 'NONE', #4371, .T. ) ;
#3851 = CYLINDRICAL_SURFACE ( 'NONE', #2201, 2.649999999999985700 ) ;
#3852 = DIRECTION ( 'NONE',  ( 6.123233995736766036E-17, -1.000000000000000000, 0.000000000000000000 ) ) ;
#3853 = EDGE_CURVE ( 'NONE', #5777, #1731, #5206, .T. ) ;
#3854 = VERTEX_POINT ( 'NONE', #5069 ) ;
#3855 = DIRECTION ( 'NONE',  ( 0.000000000000000000, 0.000000000000000000, -1.000000000000000000 ) ) ;
#3856 = VECTOR ( 'NONE', #2210, 1000.000000000000000 ) ;
#3857 = VERTEX_POINT ( 'NONE', #159 ) ;
#3858 = ORIENTED_EDGE ( 'NONE', *, *, #6230, .F. ) ;
#3859 = LINE ( 'NONE', #6757, #725 ) ;
#3860 = CARTESIAN_POINT ( 'NONE',  ( 195.0000000000000000, 8.660254037844390851, 140.0000000000000000 ) ) ;
#3861 = ITEM_DEFINED_TRANSFORMATION ( 'NONE', 'NONE', #7215,  #1963 ) ;
#3862 = DIRECTION ( 'NONE',  ( 1.000000000000000000, 0.000000000000000000, 0.000000000000000000 ) ) ;
#3863 = CARTESIAN_POINT ( 'NONE',  ( 315.0000000000000568, 8.660254037844390851, 145.0000000000000284 ) ) ;
#3864 = PRODUCT_RELATED_PRODUCT_CATEGORY ( 'part', '', ( #7153 ) ) ;
#3865 = VECTOR ( 'NONE', #3339, 1000.000000000000000 ) ;
#3866 = DIRECTION ( 'NONE',  ( -0.000000000000000000, -1.000000000000000000, -0.000000000000000000 ) ) ;
#3867 = DIRECTION ( 'NONE',  ( -1.000000000000000000, -0.000000000000000000, 0.000000000000000000 ) ) ;
#3868 = VECTOR ( 'NONE', #3038, 1000.000000000000000 ) ;
#3869 = VERTEX_POINT ( 'NONE', #1787 ) ;
#3870 = DIRECTION ( 'NONE',  ( -0.000000000000000000, -0.000000000000000000, 1.000000000000000000 ) ) ;
#3871 = DIRECTION ( 'NONE',  ( -0.000000000000000000, 1.000000000000000000, -0.000000000000000000 ) ) ;
#3872 = PRODUCT_DEFINITION_FORMATION_WITH_SPECIFIED_SOURCE ( 'ANY', '', #2469, .NOT_KNOWN. ) ;
#3873 = CIRCLE ( 'NONE', #1131, 2.649999999999985700 ) ;
#3874 = CARTESIAN_POINT ( 'NONE',  ( -2.688821387764050996E-14, -4.618802153517012954, -0.4999999999999995559 ) ) ;
#3875 = VECTOR ( 'NONE', #3172, 1000.000000000000000 ) ;
#3876 = SHAPE_DEFINITION_REPRESENTATION ( #1289, #5587 ) ;
#3877 = APPLICATION_CONTEXT ( 'automotive_design' ) ;
#3878 = VECTOR ( 'NONE', #7020, 1000.000000000000000 ) ;
#3879 = ORIENTED_EDGE ( 'NONE', *, *, #6230, .T. ) ;
#3880 = ORIENTED_EDGE ( 'NONE', *, *, #2289, .T. ) ;
#3881 = EDGE_CURVE ( 'NONE', #7016, #2247, #4451, .T. ) ;
#3882 = CARTESIAN_POINT ( 'NONE',  ( 440.0000000000000000, 0.000000000000000000, 123.0000000000000000 ) ) ;
#3883 = ORIENTED_EDGE ( 'NONE', *, *, #2190, .F. ) ;
#3884 = AXIS2_PLACEMENT_3D ( 'NONE', #714, #2347, #787 ) ;
#3885 = CARTESIAN_POINT ( 'NONE',  ( 395.0000000000000000, 8.660254037844390851, 145.0000000000000284 ) ) ;
#3886 = DIRECTION ( 'NONE',  ( -0.000000000000000000, 1.000000000000000000, 0.000000000000000000 ) ) ;
#3887 = CARTESIAN_POINT ( 'NONE',  ( 114.9999999999999858, -8.660254037844389075, 145.0000000000000284 ) ) ;
#3888 = VECTOR ( 'NONE', #4777, 1000.000000000000000 ) ;
#3889 = EDGE_LOOP ( 'NONE', ( #1119, #4269 ) ) ;
#3890 = EDGE_CURVE ( 'NONE', #432, #1772, #5166, .T. ) ;
#3891 = DIRECTION ( 'NONE',  ( 0.000000000000000000, 0.000000000000000000, 1.000000000000000000 ) ) ;
#3892 = ITEM_DEFINED_TRANSFORMATION ( 'NONE', 'NONE', #5785,  #1963 ) ;
#3893 = CARTESIAN_POINT ( 'NONE',  ( 4.999999999999999112, 8.660254037844390851, 140.0000000000000000 ) ) ;
#3894 = EDGE_CURVE ( 'NONE', #183, #3673, #3540, .T. ) ;
#3895 = COLOUR_RGB ( '',0.8941176470588234615, 0.8941176470588234615, 0.8941176470588234615 ) ;
#3896 = CARTESIAN_POINT ( 'NONE',  ( 200.0000000000000000, 0.000000000000000000, 0.000000000000000000 ) ) ;
#3897 = CIRCLE ( 'NONE', #3522, 2.649999999999985700 ) ;
#3898 = ORIENTED_EDGE ( 'NONE', *, *, #1453, .T. ) ;
#3899 = VERTEX_POINT ( 'NONE', #4784 ) ;
#3900 = ORIENTED_EDGE ( 'NONE', *, *, #1094, .T. ) ;
#3901 = ADVANCED_FACE ( 'NONE', ( #2414 ), #684, .F. ) ;
#3902 = DIRECTION ( 'NONE',  ( 0.000000000000000000, 0.000000000000000000, 1.000000000000000000 ) ) ;
#3903 = AXIS2_PLACEMENT_3D ( 'NONE', #983, #543, #6159 ) ;
#3904 = CARTESIAN_POINT ( 'NONE',  ( 2.756197834950227410, 3.027510591568626896, -3.223146290109805356 ) ) ;
#3905 = CONTEXT_DEPENDENT_SHAPE_REPRESENTATION ( #2288, #5537 ) ;
#3906 = DIRECTION ( 'NONE',  ( -0.000000000000000000, -0.000000000000000000, 1.000000000000000000 ) ) ;
#3907 = FACE_OUTER_BOUND ( 'NONE', #2115, .T. ) ;
#3908 = CARTESIAN_POINT ( 'NONE',  ( -5.000000000000000888, 8.660254037844390851, 139.9990000000000236 ) ) ;
#3909 = PRODUCT_DEFINITION_CONTEXT ( 'detailed design', #1200, 'design' ) ;
#3910 = DIRECTION ( 'NONE',  ( -0.000000000000000000, -0.000000000000000000, 1.000000000000000000 ) ) ;
#3911 =( GEOMETRIC_REPRESENTATION_CONTEXT ( 3 ) GLOBAL_UNCERTAINTY_ASSIGNED_CONTEXT ( ( #4933 ) ) GLOBAL_UNIT_ASSIGNED_CONTEXT ( ( #4749, #3567, #1376 ) ) REPRESENTATION_CONTEXT ( 'NONE', 'WORKASPACE' ) );
#3912 = ORIENTED_EDGE ( 'NONE', *, *, #2379, .T. ) ;
#3913 = FACE_OUTER_BOUND ( 'NONE', #3837, .T. ) ;
#3914 = DIRECTION ( 'NONE',  ( 0.000000000000000000, 0.000000000000000000, 1.000000000000000000 ) ) ;
#3915 = DIRECTION ( 'NONE',  ( -1.000000000000000000, 0.000000000000000000, 0.000000000000000000 ) ) ;
#3916 = FACE_BOUND ( 'NONE', #3669, .T. ) ;
#3917 =( LENGTH_UNIT ( ) NAMED_UNIT ( * ) SI_UNIT ( .MILLI., .METRE. ) );
#3918 = PLANE ( 'NONE',  #6982 ) ;
#3919 = ORIENTED_EDGE ( 'NONE', *, *, #7182, .T. ) ;
#3920 = VERTEX_POINT ( 'NONE', #229 ) ;
#3921 = CARTESIAN_POINT ( 'NONE',  ( 440.0000000000000000, 0.000000000000000000, 0.000000000000000000 ) ) ;
#3922 = ORIENTED_EDGE ( 'NONE', *, *, #96, .T. ) ;
#3923 = FACE_OUTER_BOUND ( 'NONE', #6556, .T. ) ;
#3924 = ADVANCED_FACE ( 'NONE', ( #263 ), #3045, .F. ) ;
#3925 = DIRECTION ( 'NONE',  ( 0.000000000000000000, 1.000000000000000000, 0.000000000000000000 ) ) ;
#3926 = ORIENTED_EDGE ( 'NONE', *, *, #2068, .T. ) ;
#3927 = DIRECTION ( 'NONE',  ( 0.000000000000000000, 0.000000000000000000, -1.000000000000000000 ) ) ;
#3928 = CARTESIAN_POINT ( 'NONE',  ( 53.33333333333330017, -25.00000000000000000, 162.5000000000000853 ) ) ;
#3929 = CYLINDRICAL_SURFACE ( 'NONE', #314, 2.649999999999985700 ) ;
#3930 = DIRECTION ( 'NONE',  ( 0.000000000000000000, -1.000000000000000000, 0.000000000000000000 ) ) ;
#3931 = DIRECTION ( 'NONE',  ( 0.000000000000000000, 0.000000000000000000, -1.000000000000000000 ) ) ;
#3932 = ADVANCED_FACE ( 'NONE', ( #196 ), #2967, .F. ) ;
#3933 =( REPRESENTATION_RELATIONSHIP ('NONE','NONE', #5587, #5294 ) REPRESENTATION_RELATIONSHIP_WITH_TRANSFORMATION ( #2038 )SHAPE_REPRESENTATION_RELATIONSHIP( ) );
#3934 = EDGE_LOOP ( 'NONE', ( #4210, #4198, #2047, #6430 ) ) ;
#3935 = CARTESIAN_POINT ( 'NONE',  ( 4.000000000000000000, -2.309401076758514915, -3.433295621305383349 ) ) ;
#3936 = ADVANCED_FACE ( 'NONE', ( #5347 ), #390, .T. ) ;
#3937 = ORIENTED_EDGE ( 'NONE', *, *, #1248, .F. ) ;
#3938 = ORIENTED_EDGE ( 'NONE', *, *, #3695, .T. ) ;
#3939 = CARTESIAN_POINT ( 'NONE',  ( -20.63749999999999574, 0.000000000000000000, -13.50000000000000355 ) ) ;
#3940 = CARTESIAN_POINT ( 'NONE',  ( 2.000000000000008882, 3.464101615137749945, 0.000000000000000000 ) ) ;
#3941 = ITEM_DEFINED_TRANSFORMATION ( 'NONE', 'NONE', #5093,  #1963 ) ;
#3942 = DIRECTION ( 'NONE',  ( 0.000000000000000000, 0.000000000000000000, -1.000000000000000000 ) ) ;
#3943 = DIRECTION ( 'NONE',  ( -0.000000000000000000, 1.000000000000000000, -0.000000000000000000 ) ) ;
#3944 = VERTEX_POINT ( 'NONE', #2454 ) ;
#3945 = DIRECTION ( 'NONE',  ( -1.000000000000000000, 0.000000000000000000, 0.000000000000000000 ) ) ;
#3946 = ADVANCED_FACE ( 'NONE', ( #1337 ), #3513, .F. ) ;
#3947 = ORIENTED_EDGE ( 'NONE', *, *, #1567, .F. ) ;
#3948 = CARTESIAN_POINT ( 'NONE',  ( 0.6507732100473444525, -4.243078065514795050, -0.2236248678334952777 ) ) ;
#3949 = EDGE_CURVE ( 'NONE', #6959, #2007, #6965, .T. ) ;
#3950 = CARTESIAN_POINT ( 'NONE',  ( 25.00000000000000000, 0.000000000000000000, 0.000000000000000000 ) ) ;
#3951 = DIRECTION ( 'NONE',  ( 0.000000000000000000, 0.000000000000000000, 1.000000000000000000 ) ) ;
#3952 = CARTESIAN_POINT ( 'NONE',  ( 13.50000000000000000, 1.653273178848926867E-15, -125.0000000000000000 ) ) ;
#3953 = AXIS2_PLACEMENT_3D ( 'NONE', #6407, #2344, #1886 ) ;
#3954 = FILL_AREA_STYLE ('',( #3376 ) ) ;
#3955 = ADVANCED_FACE ( 'NONE', ( #3656 ), #744, .T. ) ;
#3956 = EDGE_LOOP ( 'NONE', ( #6020, #3799, #6175, #6217, #5641, #2582 ) ) ;
#3957 = ORIENTED_EDGE ( 'NONE', *, *, #1423, .T. ) ;
#3958 = AXIS2_PLACEMENT_3D ( 'NONE', #6227, #2274, #6197 ) ;
#3959 = PRODUCT_CONTEXT ( 'NONE', #1943, 'mechanical' ) ;
#3960 = VERTEX_POINT ( 'NONE', #1273 ) ;
#3961 = DIRECTION ( 'NONE',  ( 0.000000000000000000, 0.000000000000000000, -1.000000000000000000 ) ) ;
#3962 = ADVANCED_FACE ( 'NONE', ( #5956 ), #303, .F. ) ;
#3963 = AXIS2_PLACEMENT_3D ( 'NONE', #1551, #993, #2016 ) ;
#3964 = PLANE ( 'NONE',  #4626 ) ;
#3965 = VERTEX_POINT ( 'NONE', #463 ) ;
#3966 = CARTESIAN_POINT ( 'NONE',  ( -4.000000000000000000, 2.309401076758498483, -5.000000000000000000 ) ) ;
#3967 = AXIS2_PLACEMENT_3D ( 'NONE', #2283, #587, #1764 ) ;
#3968 = FACE_OUTER_BOUND ( 'NONE', #667, .T. ) ;
#3969 = CARTESIAN_POINT ( 'NONE',  ( -5.000000000000000888, 8.660254037844390851, 145.0000000000000284 ) ) ;
#3970 = DIRECTION ( 'NONE',  ( 1.000000000000000000, 0.000000000000000000, 0.000000000000000000 ) ) ;
#3971 = ORIENTED_EDGE ( 'NONE', *, *, #2721, .T. ) ;
#3972 = CARTESIAN_POINT ( 'NONE',  ( 235.0000000000000000, 8.660254037844390851, 140.0000000000000000 ) ) ;
#3973 = EDGE_CURVE ( 'NONE', #4758, #6476, #2125, .T. ) ;
#3974 = ORIENTED_EDGE ( 'NONE', *, *, #5933, .T. ) ;
#3975 = DIRECTION ( 'NONE',  ( 0.000000000000000000, 0.000000000000000000, 1.000000000000000000 ) ) ;
#3976 = DIRECTION ( 'NONE',  ( 0.000000000000000000, 1.000000000000000000, 0.000000000000000000 ) ) ;
#3977 = CONTEXT_DEPENDENT_SHAPE_REPRESENTATION ( #7135, #6474 ) ;
#3978 = CARTESIAN_POINT ( 'NONE',  ( 35.00000000000000000, 8.660254037844390851, 145.0000000000000284 ) ) ;
#3979 = DIRECTION ( 'NONE',  ( -0.000000000000000000, -0.000000000000000000, -1.000000000000000000 ) ) ;
#3980 = ORIENTED_EDGE ( 'NONE', *, *, #4529, .T. ) ;
#3981 = CARTESIAN_POINT ( 'NONE',  ( -13.50000000000000000, 0.000000000000000000, -125.0000000000000000 ) ) ;
#3982 = VERTEX_POINT ( 'NONE', #1448 ) ;
#3983 = CARTESIAN_POINT ( 'NONE',  ( -1.999999999999998668, 0.000000000000000000, -10.20000000000000107 ) ) ;
#3984 = CARTESIAN_POINT ( 'NONE',  ( -2.807080416178626692, 3.225969019225154444, -3.502507215260441065 ) ) ;
#3985 = DIRECTION ( 'NONE',  ( 0.000000000000000000, 1.000000000000000000, 0.000000000000000000 ) ) ;
#3986 = DIRECTION ( 'NONE',  ( 0.000000000000000000, 0.000000000000000000, -1.000000000000000000 ) ) ;
#3987 = ADVANCED_FACE ( 'NONE', ( #5578 ), #3810, .F. ) ;
#3988 = AXIS2_PLACEMENT_3D ( 'NONE', #879, #4968, #7255 ) ;
#3989 = AXIS2_PLACEMENT_3D ( 'NONE', #6427, #5249, #5392 ) ;
#3990 = AXIS2_PLACEMENT_3D ( 'NONE', #1057, #2162, #4534 ) ;
#3991 = ORIENTED_EDGE ( 'NONE', *, *, #54, .T. ) ;
#3992 = VECTOR ( 'NONE', #2137, 1000.000000000000000 ) ;
#3993 = AXIS2_PLACEMENT_3D ( 'NONE', #5507, #1585, #950 ) ;
#3994 = DIRECTION ( 'NONE',  ( -1.000000000000000000, 0.000000000000000000, 0.000000000000000000 ) ) ;
#3995 = ORIENTED_EDGE ( 'NONE', *, *, #2647, .F. ) ;
#3996 = ADVANCED_FACE ( 'NONE', ( #5490 ), #973, .T. ) ;
#3997 = FACE_BOUND ( 'NONE', #6756, .T. ) ;
#3998 = PRODUCT_DEFINITION_FORMATION_WITH_SPECIFIED_SOURCE ( 'ANY', '', #870, .NOT_KNOWN. ) ;
#3999 = VECTOR ( 'NONE', #1928, 1000.000000000000000 ) ;
#4000 = DIRECTION ( 'NONE',  ( 0.000000000000000000, 0.000000000000000000, -1.000000000000000000 ) ) ;
#4001 = ORIENTED_EDGE ( 'NONE', *, *, #2046, .T. ) ;
#4002 = AXIS2_PLACEMENT_3D ( 'NONE', #3374, #2220, #3337 ) ;
#4003 =( GEOMETRIC_REPRESENTATION_CONTEXT ( 3 ) GLOBAL_UNCERTAINTY_ASSIGNED_CONTEXT ( ( #3292 ) ) GLOBAL_UNIT_ASSIGNED_CONTEXT ( ( #1555, #2870, #2315 ) ) REPRESENTATION_CONTEXT ( 'NONE', 'WORKASPACE' ) );
#4004 = CARTESIAN_POINT ( 'NONE',  ( 3.999999999999998224, 2.472263674411418588, -3.687027874309861897 ) ) ;
#4005 = DIRECTION ( 'NONE',  ( -1.000000000000000000, 0.000000000000000000, 0.000000000000000000 ) ) ;
#4006 = CARTESIAN_POINT ( 'NONE',  ( 160.0000000000000000, 0.000000000000000000, 123.0000000000000000 ) ) ;
#4007 = EDGE_LOOP ( 'NONE', ( #1577, #312 ) ) ;
#4008 = AXIS2_PLACEMENT_3D ( 'NONE', #6481, #5920, #4077 ) ;
#4009 = CARTESIAN_POINT ( 'NONE',  ( -4.197393957002303999, -7.773935952363655451E-14, -3.503767560748929810 ) ) ;
#4010 = AXIS2_PLACEMENT_3D ( 'NONE', #2195, #6785, #1644 ) ;
#4011 = VERTEX_POINT ( 'NONE', #1534 ) ;
#4012 = DIRECTION ( 'NONE',  ( -0.000000000000000000, -0.000000000000000000, -1.000000000000000000 ) ) ;
#4013 = CARTESIAN_POINT ( 'NONE',  ( 0.000000000000000000, 0.000000000000000000, -140.0000000000000000 ) ) ;
#4014 = VECTOR ( 'NONE', #4455, 1000.000000000000000 ) ;
#4015 = CONTEXT_DEPENDENT_SHAPE_REPRESENTATION ( #2152, #5333 ) ;
#4016 = CARTESIAN_POINT ( 'NONE',  ( 2.000000000000000444, 3.464101615137754830, -3.142992957459231018 ) ) ;
#4017 = FACE_OUTER_BOUND ( 'NONE', #1434, .T. ) ;
#4018 = CIRCLE ( 'NONE', #5570, 10.00000000000000000 ) ;
#4019 = VERTEX_POINT ( 'NONE', #7112 ) ;
#4020 = DIRECTION ( 'NONE',  ( 0.000000000000000000, 0.000000000000000000, -1.000000000000000000 ) ) ;
#4021 = EDGE_CURVE ( 'NONE', #2157, #6398, #4895, .T. ) ;
#4022 = ORIENTED_EDGE ( 'NONE', *, *, #735, .F. ) ;
#4023 = PRODUCT_DEFINITION_SHAPE ( 'NONE', 'NONE',  #7399 ) ;
#4024 = CARTESIAN_POINT ( 'NONE',  ( 365.0000000000000000, 8.660254037844390851, 139.9990000000000236 ) ) ;
#4025 = CARTESIAN_POINT ( 'NONE',  ( -3.522875095019672109, 2.820352903225427532, -3.598441714920591394 ) ) ;
#4026 = CARTESIAN_POINT ( 'NONE',  ( -2.499999999999999556, 3.061616997868382648E-16, 3.469446951953614189E-15 ) ) ;
#4027 = VECTOR ( 'NONE', #771, 1000.000000000000000 ) ;
#4028 = CARTESIAN_POINT ( 'NONE',  ( -3.999999999999999112, 1.539600717838996324, -3.300726591567078039 ) ) ;
#4029 = ADVANCED_FACE ( 'NONE', ( #896 ), #154, .T. ) ;
#4030 = ORIENTED_EDGE ( 'NONE', *, *, #3832, .F. ) ;
#4031 = ORIENTED_EDGE ( 'NONE', *, *, #5545, .F. ) ;
#4032 = LINE ( 'NONE', #597, #1385 ) ;
#4033 = ADVANCED_FACE ( 'NONE', ( #5455 ), #1495, .F. ) ;
#4034 = ORIENTED_EDGE ( 'NONE', *, *, #746, .F. ) ;
#4035 = CARTESIAN_POINT ( 'NONE',  ( 136.6666666666666288, -25.00000000000000000, 162.5000000000000853 ) ) ;
#4036 = ORIENTED_EDGE ( 'NONE', *, *, #5712, .T. ) ;
#4037 = DIRECTION ( 'NONE',  ( 0.000000000000000000, -1.000000000000000000, 0.000000000000000000 ) ) ;
#4038 = PLANE ( 'NONE',  #2979 ) ;
#4039 = ORIENTED_EDGE ( 'NONE', *, *, #3578, .F. ) ;
#4040 = CARTESIAN_POINT ( 'NONE',  ( -4.000000000000000000, 2.309401076758498483, -0.4999999999999927280 ) ) ;
#4041 = LINE ( 'NONE', #683, #913 ) ;
#4042 = CONTEXT_DEPENDENT_SHAPE_REPRESENTATION ( #1998, #2447 ) ;
#4043 = CYLINDRICAL_SURFACE ( 'NONE', #4200, 2.649999999999985700 ) ;
#4044 = CARTESIAN_POINT ( 'NONE',  ( -20.63749999999999574, 0.000000000000000000, -12.77499999999999858 ) ) ;
#4045 = ADVANCED_FACE ( 'NONE', ( #2684 ), #3275, .T. ) ;
#4046 = ORIENTED_EDGE ( 'NONE', *, *, #2728, .T. ) ;
#4047 = DIRECTION ( 'NONE',  ( 1.000000000000000000, 0.000000000000000000, 0.000000000000000000 ) ) ;
#4048 = VERTEX_POINT ( 'NONE', #5990 ) ;
#4049 = PLANE ( 'NONE',  #382 ) ;
#4050 = CARTESIAN_POINT ( 'NONE',  ( -2.725741868435985094, 3.045094352034055429, -3.220599429844047012 ) ) ;
#4051 = LINE ( 'NONE', #6239, #373 ) ;
#4052 = LINE ( 'NONE', #1183, #4711 ) ;
#4053 = FACE_OUTER_BOUND ( 'NONE', #7266, .T. ) ;
#4054 = VERTEX_POINT ( 'NONE', #7148 ) ;
#4055 = ORIENTED_EDGE ( 'NONE', *, *, #5724, .F. ) ;
#4056 = APPLICATION_PROTOCOL_DEFINITION ( 'draft international standard', 'automotive_design', 1998, #7329 ) ;
#4057 = EDGE_LOOP ( 'NONE', ( #5438, #2658, #5224, #4991 ) ) ;
#4058 = ADVANCED_FACE ( 'NONE', ( #4296, #3772 ), #4986, .F. ) ;
#4059 = EDGE_CURVE ( 'NONE', #7144, #4178, #4380, .T. ) ;
#4060 = CARTESIAN_POINT ( 'NONE',  ( 2.100000000000000089, 0.000000000000000000, -5.000000000000000000 ) ) ;
#4061 = ORIENTED_EDGE ( 'NONE', *, *, #1321, .T. ) ;
#4062 =( REPRESENTATION_RELATIONSHIP ('NONE','NONE', #5587, #6025 ) REPRESENTATION_RELATIONSHIP_WITH_TRANSFORMATION ( #5170 )SHAPE_REPRESENTATION_RELATIONSHIP( ) );
#4063 = SURFACE_STYLE_FILL_AREA ( #1777 ) ;
#4064 = LINE ( 'NONE', #1778, #2208 ) ;
#4065 = ADVANCED_FACE ( 'NONE', ( #3850 ), #3107, .F. ) ;
#4066 = EDGE_LOOP ( 'NONE', ( #2932, #6715, #5046, #3559 ) ) ;
#4067 = PRODUCT_DEFINITION_SHAPE ( 'NONE', 'NONE',  #7384 ) ;
#4068 = DIRECTION ( 'NONE',  ( 1.000000000000000000, 0.000000000000000000, 0.000000000000000000 ) ) ;
#4069 = CIRCLE ( 'NONE', #5382, 2.649999999999985700 ) ;
#4070 = ORIENTED_EDGE ( 'NONE', *, *, #6559, .T. ) ;
#4071 = AXIS2_PLACEMENT_3D ( 'NONE', #5595, #3827, #1469 ) ;
#4072 = VERTEX_POINT ( 'NONE', #6146 ) ;
#4073 = DIRECTION ( 'NONE',  ( 0.000000000000000000, -0.000000000000000000, -1.000000000000000000 ) ) ;
#4074 = DIRECTION ( 'NONE',  ( 1.000000000000000000, 0.000000000000000000, 0.000000000000000000 ) ) ;
#4075 = CONTEXT_DEPENDENT_SHAPE_REPRESENTATION ( #4062, #2973 ) ;
#4076 = CARTESIAN_POINT ( 'NONE',  ( 2.725741868436127202, -3.045094352033990148, -3.220599429844051453 ) ) ;
#4077 = DIRECTION ( 'NONE',  ( 1.000000000000000000, 0.000000000000000000, 0.000000000000000000 ) ) ;
#4078 = EDGE_CURVE ( 'NONE', #214, #1606, #1016, .T. ) ;
#4079 = ORIENTED_EDGE ( 'NONE', *, *, #1823, .F. ) ;
#4080 = DIRECTION ( 'NONE',  ( -0.000000000000000000, 1.000000000000000000, -0.000000000000000000 ) ) ;
#4081 = EDGE_LOOP ( 'NONE', ( #6931, #3555, #2291, #2834 ) ) ;
#4082 = PRODUCT_RELATED_PRODUCT_CATEGORY ( 'part', '', ( #3544 ) ) ;
#4083 = CARTESIAN_POINT ( 'NONE',  ( 275.0000000000000000, -8.660254037844389075, 140.0000000000000000 ) ) ;
#4084 = LINE ( 'NONE', #6380, #3279 ) ;
#4085 = LINE ( 'NONE', #4549, #2501 ) ;
#4086 = CARTESIAN_POINT ( 'NONE',  ( -1.317756351988340180, 3.857995168970202116, -0.04852650426601388955 ) ) ;
#4087 = VECTOR ( 'NONE', #3906, 1000.000000000000000 ) ;
#4088 = DIRECTION ( 'NONE',  ( 0.000000000000000000, 0.000000000000000000, 1.000000000000000000 ) ) ;
#4089 = EDGE_LOOP ( 'NONE', ( #2953, #3024, #1025, #6359 ) ) ;
#4090 = ORIENTED_EDGE ( 'NONE', *, *, #5913, .T. ) ;
#4091 = CONTEXT_DEPENDENT_SHAPE_REPRESENTATION ( #2772, #7213 ) ;
#4092 = VECTOR ( 'NONE', #3235, 1000.000000000000000 ) ;
#4093 = DIRECTION ( 'NONE',  ( 0.000000000000000000, 1.000000000000000000, 0.000000000000000000 ) ) ;
#4094 = ORIENTED_EDGE ( 'NONE', *, *, #96, .F. ) ;
#4095 = SURFACE_SIDE_STYLE ('',( #6950 ) ) ;
#4096 = VECTOR ( 'NONE', #516, 1000.000000000000000 ) ;
#4097 = AXIS2_PLACEMENT_3D ( 'NONE', #4336, #1498, #3775 ) ;
#4098 = DIRECTION ( 'NONE',  ( 0.000000000000000000, -1.000000000000000000, 0.000000000000000000 ) ) ;
#4099 = ADVANCED_FACE ( 'NONE', ( #1416 ), #2639, .F. ) ;
#4100 = ORIENTED_EDGE ( 'NONE', *, *, #2104, .T. ) ;
#4101 = EDGE_CURVE ( 'NONE', #1241, #3638, #2984, .T. ) ;
#4102 = AXIS2_PLACEMENT_3D ( 'NONE', #6019, #6662, #5567 ) ;
#4103 = DIRECTION ( 'NONE',  ( 1.000000000000000000, 0.000000000000000000, 0.000000000000000000 ) ) ;
#4104 = CIRCLE ( 'NONE', #1826, 4.250000000000000000 ) ;
#4105 = VECTOR ( 'NONE', #4787, 1000.000000000000000 ) ;
#4106 = LINE ( 'NONE', #6437, #3868 ) ;
#4107 = FILL_AREA_STYLE_COLOUR ( '', #31 ) ;
#4108 =( REPRESENTATION_RELATIONSHIP ('NONE','NONE', #5587, #3270 ) REPRESENTATION_RELATIONSHIP_WITH_TRANSFORMATION ( #7025 )SHAPE_REPRESENTATION_RELATIONSHIP( ) );
#4109 = ORIENTED_EDGE ( 'NONE', *, *, #3418, .F. ) ;
#4110 = AXIS2_PLACEMENT_3D ( 'NONE', #1719, #1299, #1228 ) ;
#4111 = EDGE_CURVE ( 'NONE', #5639, #1932, #7324, .T. ) ;
#4112 = EDGE_CURVE ( 'NONE', #3509, #6334, #812, .T. ) ;
#4113 = DIRECTION ( 'NONE',  ( 0.000000000000000000, 0.000000000000000000, -1.000000000000000000 ) ) ;
#4114 = DIRECTION ( 'NONE',  ( 0.000000000000000000, 0.000000000000000000, -1.000000000000000000 ) ) ;
#4115 = CARTESIAN_POINT ( 'NONE',  ( 0.000000000000000000, 15.00000000000000000, 145.0000000000000284 ) ) ;
#4116 = DIRECTION ( 'NONE',  ( -0.000000000000000000, 1.000000000000000000, 0.000000000000000000 ) ) ;
#4117 = VECTOR ( 'NONE', #2485, 1000.000000000000000 ) ;
#4118 =( NAMED_UNIT ( * ) PLANE_ANGLE_UNIT ( ) SI_UNIT ( $, .RADIAN. ) );
#4119 = AXIS2_PLACEMENT_3D ( 'NONE', #6482, #5240, #5316 ) ;
#4120 = ORIENTED_EDGE ( 'NONE', *, *, #6581, .F. ) ;
#4121 = FACE_OUTER_BOUND ( 'NONE', #904, .T. ) ;
#4122 = EDGE_CURVE ( 'NONE', #380, #5828, #855, .T. ) ;
#4123 = VERTEX_POINT ( 'NONE', #4849 ) ;
#4124 = VECTOR ( 'NONE', #7305, 1000.000000000000000 ) ;
#4125 = ORIENTED_EDGE ( 'NONE', *, *, #5906, .T. ) ;
#4126 = DIRECTION ( 'NONE',  ( -0.000000000000000000, -0.000000000000000000, 1.000000000000000000 ) ) ;
#4127 = CYLINDRICAL_SURFACE ( 'NONE', #4616, 4.250000000000000000 ) ;
#4128 = CARTESIAN_POINT ( 'NONE',  ( 285.0000000000000568, 8.660254037844390851, 140.0000000000000000 ) ) ;
#4129 = DIRECTION ( 'NONE',  ( 1.000000000000000000, 0.000000000000000000, 0.000000000000000000 ) ) ;
#4130 = VECTOR ( 'NONE', #2751, 1000.000000000000000 ) ;
#4131 = DIRECTION ( 'NONE',  ( -0.000000000000000000, -0.000000000000000000, 1.000000000000000000 ) ) ;
#4132 = VECTOR ( 'NONE', #6170, 1000.000000000000000 ) ;
#4133 = EDGE_LOOP ( 'NONE', ( #343, #1742, #2204, #466 ) ) ;
#4134 = ORIENTED_EDGE ( 'NONE', *, *, #2451, .F. ) ;
#4135 = CYLINDRICAL_SURFACE ( 'NONE', #4010, 2.649999999999985700 ) ;
#4136 = ORIENTED_EDGE ( 'NONE', *, *, #2234, .T. ) ;
#4137 = VECTOR ( 'NONE', #3783, 1000.000000000000000 ) ;
#4138 =( LENGTH_UNIT ( ) NAMED_UNIT ( * ) SI_UNIT ( .MILLI., .METRE. ) );
#4139 = CARTESIAN_POINT ( 'NONE',  ( 53.33333333333330017, -25.00000000000000000, -165.1500000000000625 ) ) ;
#4140 = AXIS2_PLACEMENT_3D ( 'NONE', #415, #5373, #6142 ) ;
#4141 = ORIENTED_EDGE ( 'NONE', *, *, #1248, .T. ) ;
#4142 = ADVANCED_FACE ( 'NONE', ( #2706 ), #4776, .F. ) ;
#4143 = CARTESIAN_POINT ( 'NONE',  ( 386.6666666666666288, -15.00000000000000000, 159.8500000000001080 ) ) ;
#4144 = DIRECTION ( 'NONE',  ( 1.000000000000000000, 0.000000000000000000, 0.000000000000000000 ) ) ;
#4145 = DIRECTION ( 'NONE',  ( 0.000000000000000000, 0.000000000000000000, 1.000000000000000000 ) ) ;
#4146 = ORIENTED_EDGE ( 'NONE', *, *, #6333, .T. ) ;
#4147 = DIRECTION ( 'NONE',  ( 1.000000000000000000, 0.000000000000000000, 0.000000000000000000 ) ) ;
#4148 = ADVANCED_FACE ( 'NONE', ( #6771, #6209 ), #1371, .T. ) ;
#4149 = ITEM_DEFINED_TRANSFORMATION ( 'NONE', 'NONE', #2802,  #1963 ) ;
#4150 = CARTESIAN_POINT ( 'NONE',  ( 75.00000000000001421, 8.660254037844390851, 139.9990000000000236 ) ) ;
#4151 = DIRECTION ( 'NONE',  ( 0.5000000000000013323, -0.8660254037844379305, 0.000000000000000000 ) ) ;
#4152 = EDGE_CURVE ( 'NONE', #1397, #6725, #5948, .T. ) ;
#4153 = ORIENTED_EDGE ( 'NONE', *, *, #6741, .F. ) ;
#4154 = DIRECTION ( 'NONE',  ( 0.000000000000000000, 0.000000000000000000, 1.000000000000000000 ) ) ;
#4155 = PRODUCT ( 'side rail', 'side rail', '', ( #5225 ) ) ;
#4156 = MECHANICAL_DESIGN_GEOMETRIC_PRESENTATION_REPRESENTATION (  '', ( #1839 ), #170 ) ;
#4157 = VERTEX_POINT ( 'NONE', #3336 ) ;
#4158 = ORIENTED_EDGE ( 'NONE', *, *, #6699, .F. ) ;
#4159 = LINE ( 'NONE', #6938, #4915 ) ;
#4160 = CARTESIAN_POINT ( 'NONE',  ( -3.472371940586054251, -2.614027278893156669, -3.320322319202162031 ) ) ;
#4161 = CARTESIAN_POINT ( 'NONE',  ( -20.63749999999999929, 0.000000000000000000, 0.000000000000000000 ) ) ;
#4162 = FACE_OUTER_BOUND ( 'NONE', #6506, .T. ) ;
#4163 = EDGE_CURVE ( 'NONE', #3217, #2273, #1108, .T. ) ;
#4164 = DIRECTION ( 'NONE',  ( 0.000000000000000000, -1.000000000000000000, 0.000000000000000000 ) ) ;
#4165 = DIRECTION ( 'NONE',  ( 1.000000000000000000, 0.000000000000000000, 0.000000000000000000 ) ) ;
#4166 = EDGE_LOOP ( 'NONE', ( #6196, #779, #3380, #3858 ) ) ;
#4167 = ORIENTED_EDGE ( 'NONE', *, *, #2225, .T. ) ;
#4168 = LINE ( 'NONE', #6431, #1475 ) ;
#4169 = ORIENTED_EDGE ( 'NONE', *, *, #2101, .F. ) ;
#4170 = ADVANCED_FACE ( 'NONE', ( #3254 ), #5006, .F. ) ;
#4171 = EDGE_CURVE ( 'NONE', #7081, #6352, #7066, .T. ) ;
#4172 = FACE_OUTER_BOUND ( 'NONE', #2132, .T. ) ;
#4173 = ORIENTED_EDGE ( 'NONE', *, *, #5103, .F. ) ;
#4174 = EDGE_CURVE ( 'NONE', #2423, #5618, #30, .T. ) ;
#4175 = DIRECTION ( 'NONE',  ( -0.000000000000000000, -0.000000000000000000, 1.000000000000000000 ) ) ;
#4176 = DIRECTION ( 'NONE',  ( 1.000000000000000000, 0.000000000000000000, 0.000000000000000000 ) ) ;
#4177 = CARTESIAN_POINT ( 'NONE',  ( 0.000000000000000000, 0.000000000000000000, 140.0000000000000000 ) ) ;
#4178 = VERTEX_POINT ( 'NONE', #4808 ) ;
#4179 = AXIS2_PLACEMENT_3D ( 'NONE', #4462, #1686, #1654 ) ;
#4180 = LINE ( 'NONE', #6479, #2786 ) ;
#4181 = CARTESIAN_POINT ( 'NONE',  ( 2.712762565639649015, -3.052587955997662306, -3.430618716626630871 ) ) ;
#4182 = DIRECTION ( 'NONE',  ( 0.8660254037844379305, 0.5000000000000013323, 0.000000000000000000 ) ) ;
#4183 = PRESENTATION_STYLE_ASSIGNMENT (( #823 ) ) ;
#4184 = VERTEX_POINT ( 'NONE', #6728 ) ;
#4185 = CARTESIAN_POINT ( 'NONE',  ( 303.3333333333333144, -20.00000000000000000, 162.5000000000000853 ) ) ;
#4186 = VECTOR ( 'NONE', #2219, 1000.000000000000114 ) ;
#4187 = EDGE_CURVE ( 'NONE', #763, #1987, #2752, .T. ) ;
#4188 = ORIENTED_EDGE ( 'NONE', *, *, #193, .F. ) ;
#4189 = PRODUCT_DEFINITION_SHAPE ( 'NONE', 'NONE',  #7394 ) ;
#4190 = ORIENTED_EDGE ( 'NONE', *, *, #7182, .F. ) ;
#4191 = DIRECTION ( 'NONE',  ( 1.000000000000000000, 0.000000000000000000, 0.000000000000000000 ) ) ;
#4192 = CARTESIAN_POINT ( 'NONE',  ( -4.140404888673278272, -2.228338276487456415, -3.686887068327035166 ) ) ;
#4193 = DIRECTION ( 'NONE',  ( 0.000000000000000000, 0.000000000000000000, -1.000000000000000000 ) ) ;
#4194 = DIRECTION ( 'NONE',  ( 0.000000000000000000, 0.000000000000000000, -1.000000000000000000 ) ) ;
#4195 = CIRCLE ( 'NONE', #979, 2.649999999999985700 ) ;
#4196 = CARTESIAN_POINT ( 'NONE',  ( 114.9999999999999858, -8.660254037844389075, 139.9990000000000236 ) ) ;
#4197 = CARTESIAN_POINT ( 'NONE',  ( -30.00000000000002842, -20.00000000000000000, 140.0000000000000000 ) ) ;
#4198 = ORIENTED_EDGE ( 'NONE', *, *, #4502, .T. ) ;
#4199 = EDGE_CURVE ( 'NONE', #2725, #1422, #1039, .T. ) ;
#4200 = AXIS2_PLACEMENT_3D ( 'NONE', #582, #2868, #2838 ) ;
#4201 = CONTEXT_DEPENDENT_SHAPE_REPRESENTATION ( #4873, #3112 ) ;
#4202 = CARTESIAN_POINT ( 'NONE',  ( 3.510273485745307731, 2.827716139362654424, -3.610536846335885564 ) ) ;
#4203 = VERTEX_POINT ( 'NONE', #481 ) ;
#4204 =( REPRESENTATION_RELATIONSHIP ('NONE','NONE', #5587, #5294 ) REPRESENTATION_RELATIONSHIP_WITH_TRANSFORMATION ( #3809 )SHAPE_REPRESENTATION_RELATIONSHIP( ) );
#4205 = VECTOR ( 'NONE', #1348, 1000.000000000000000 ) ;
#4206 = FACE_BOUND ( 'NONE', #6336, .T. ) ;
#4207 = UNCERTAINTY_MEASURE_WITH_UNIT (LENGTH_MEASURE( 1.000000000000000082E-05 ), #2145, 'distance_accuracy_value', 'NONE');
#4208 = ORIENTED_EDGE ( 'NONE', *, *, #2527, .F. ) ;
#4209 = EDGE_CURVE ( 'NONE', #1367, #3461, #5980, .T. ) ;
#4210 = ORIENTED_EDGE ( 'NONE', *, *, #746, .T. ) ;
#4211 = CARTESIAN_POINT ( 'NONE',  ( 0.7826237921249277196, 0.000000000000000000, 0.000000000000000000 ) ) ;
#4212 = PRODUCT_DEFINITION_SHAPE ( 'NONE', 'NONE',  #7341 ) ;
#4213 = LINE ( 'NONE', #4373, #1497 ) ;
#4214 = ORIENTED_EDGE ( 'NONE', *, *, #4404, .F. ) ;
#4215 = DIRECTION ( 'NONE',  ( -1.000000000000000000, -0.000000000000000000, -0.000000000000000000 ) ) ;
#4216 = ORIENTED_EDGE ( 'NONE', *, *, #4356, .F. ) ;
#4217 = AXIS2_PLACEMENT_3D ( 'NONE', #6102, #5445, #1440 ) ;
#4218 = AXIS2_PLACEMENT_3D ( 'NONE', #2655, #3866, #354 ) ;
#4219 = AXIS2_PLACEMENT_3D ( 'NONE', #3966, #699, #6252 ) ;
#4220 = CARTESIAN_POINT ( 'NONE',  ( 4.203935335434060505, 1.640780671294165272, -3.598452447879202598 ) ) ;
#4221 = CONTEXT_DEPENDENT_SHAPE_REPRESENTATION ( #5452, #1386 ) ;
#4222 = CARTESIAN_POINT ( 'NONE',  ( 2.807080416178989513, -3.225969019225150003, -3.502507215260505014 ) ) ;
#4223 = CYLINDRICAL_SURFACE ( 'NONE', #4231, 13.50000000000000355 ) ;
#4224 = ORIENTED_EDGE ( 'NONE', *, *, #1925, .F. ) ;
#4225 = CIRCLE ( 'NONE', #4480, 1.050000000000000488 ) ;
#4226 = CARTESIAN_POINT ( 'NONE',  ( -3.861362476283256129, -2.629030857716004199, -3.671615880910374941 ) ) ;
#4227 = ORIENTED_EDGE ( 'NONE', *, *, #3712, .T. ) ;
#4228 = VERTEX_POINT ( 'NONE', #6171 ) ;
#4229 = DIRECTION ( 'NONE',  ( 0.000000000000000000, 0.000000000000000000, -1.000000000000000000 ) ) ;
#4230 = CARTESIAN_POINT ( 'NONE',  ( 435.0000000000000568, -8.660254037844389075, 145.0000000000000284 ) ) ;
#4231 = AXIS2_PLACEMENT_3D ( 'NONE', #6520, #1888, #1381 ) ;
#4232 = PRESENTATION_LAYER_ASSIGNMENT (  '', '', ( #670 ) ) ;
#4233 = FACE_OUTER_BOUND ( 'NONE', #3444, .T. ) ;
#4234 = LINE ( 'NONE', #4794, #3878 ) ;
#4235 = EDGE_CURVE ( 'NONE', #1606, #853, #2025, .T. ) ;
#4236 = CARTESIAN_POINT ( 'NONE',  ( 219.9999999999999716, -15.00000000000000000, 162.5000000000000853 ) ) ;
#4237 = CARTESIAN_POINT ( 'NONE',  ( -20.63749999999999574, 0.000000000000000000, 0.000000000000000000 ) ) ;
#4238 = VECTOR ( 'NONE', #6189, 1000.000000000000000 ) ;
#4239 = ORIENTED_EDGE ( 'NONE', *, *, #5485, .F. ) ;
#4240 = CARTESIAN_POINT ( 'NONE',  ( 1.411581201560190495E-15, 4.862606272033091592, -3.745885042887436622 ) ) ;
#4241 = EDGE_LOOP ( 'NONE', ( #1001, #4136, #3237, #2405 ) ) ;
#4242 = CARTESIAN_POINT ( 'NONE',  ( 1.734723475976807094E-15, 4.618802153517012954, -0.4999999999999995559 ) ) ;
#4243 =( BOUNDED_SURFACE ( )  B_SPLINE_SURFACE ( 3, 2, ( 
 ( #3325, #2050, #386 ),
 ( #6198, #1580, #504 ),
 ( #3904, #2649, #4348 ),
 ( #1028, #1064, #4951 ),
 ( #2207, #7236, #3201 ),
 ( #1096, #6758, #2167 ) ),
 .UNSPECIFIED., .F., .F., .F. ) 
 B_SPLINE_SURFACE_WITH_KNOTS ( ( 4, 2, 4 ),
 ( 3, 3 ),
 ( 0.02032853247518126225, 0.02278863295364821212, 0.02524873343211516200 ),
 ( 0.000000000000000000, 1.000000000000000000 ),
 .UNSPECIFIED. ) 
 GEOMETRIC_REPRESENTATION_ITEM ( )  RATIONAL_B_SPLINE_SURFACE ( (
 ( 1.000000000000000000, 0.8047781615896835161, 1.000000000000000000),
 ( 1.000000000000000000, 0.8123767586291043008, 1.000000000000000000),
 ( 1.000000000000000000, 0.8190662415562011134, 1.000000000000000000),
 ( 1.000000000000000000, 0.8192361015671398849, 1.000000000000000000),
 ( 1.000000000000000000, 0.8126135807102121689, 1.000000000000000000),
 ( 1.000000000000000000, 0.8047712338318585568, 1.000000000000000000) ) ) 
 REPRESENTATION_ITEM ( '' )  SURFACE ( )  );
#4244 = AXIS2_PLACEMENT_3D ( 'NONE', #6104, #6509, #3647 ) ;
#4245 = SURFACE_SIDE_STYLE ('',( #5976 ) ) ;
#4246 = VECTOR ( 'NONE', #1522, 1000.000000000000000 ) ;
#4247 = EDGE_CURVE ( 'NONE', #4184, #1241, #3282, .T. ) ;
#4248 = CARTESIAN_POINT ( 'NONE',  ( 0.000000000000000000, 0.000000000000000000, 140.0000000000000000 ) ) ;
#4249 = ORIENTED_EDGE ( 'NONE', *, *, #418, .F. ) ;
#4250 = AXIS2_PLACEMENT_3D ( 'NONE', #2345, #7007, #4716 ) ;
#4251 = ORIENTED_EDGE ( 'NONE', *, *, #5997, .T. ) ;
#4252 = APPLICATION_CONTEXT ( 'automotive_design' ) ;
#4253 = DIRECTION ( 'NONE',  ( 0.000000000000000000, 1.000000000000000000, 0.000000000000000000 ) ) ;
#4254 = CARTESIAN_POINT ( 'NONE',  ( 0.000000000000000000, 15.00000000000000000, 140.0000000000000000 ) ) ;
#4255 = EDGE_CURVE ( 'NONE', #3309, #6561, #514, .T. ) ;
#4256 = AXIS2_PLACEMENT_3D ( 'NONE', #1010, #6892, #1748 ) ;
#4257 = DIRECTION ( 'NONE',  ( 1.000000000000000000, 0.000000000000000000, 0.000000000000000000 ) ) ;
#4258 = PLANE ( 'NONE',  #4514 ) ;
#4259 = ORIENTED_EDGE ( 'NONE', *, *, #2149, .T. ) ;
#4260 = EDGE_CURVE ( 'NONE', #1596, #6322, #5505, .T. ) ;
#4261 = DIRECTION ( 'NONE',  ( -0.000000000000000000, -0.000000000000000000, 1.000000000000000000 ) ) ;
#4262 = DIRECTION ( 'NONE',  ( 0.000000000000000000, 1.000000000000000000, 0.000000000000000000 ) ) ;
#4263 = DIRECTION ( 'NONE',  ( 0.000000000000000000, 0.000000000000000000, 1.000000000000000000 ) ) ;
#4264 = CARTESIAN_POINT ( 'NONE',  ( 303.3333333333333144, -10.00000000000000000, 162.5000000000000853 ) ) ;
#4265 = COLOUR_RGB ( '',1.000000000000000000, 0.9490196078431372140, 0.9098039215686274384 ) ;
#4266 = EDGE_LOOP ( 'NONE', ( #4802, #2500, #1685 ) ) ;
#4267 = DIRECTION ( 'NONE',  ( 1.000000000000000000, 0.000000000000000000, 0.000000000000000000 ) ) ;
#4268 = VERTEX_POINT ( 'NONE', #6347 ) ;
#4269 = ORIENTED_EDGE ( 'NONE', *, *, #521, .F. ) ;
#4270 = FACE_OUTER_BOUND ( 'NONE', #5105, .T. ) ;
#4271 = CARTESIAN_POINT ( 'NONE',  ( 4.999999999999999112, -8.660254037844389075, 140.0000000000000000 ) ) ;
#4272 = CARTESIAN_POINT ( 'NONE',  ( 0.000000000000000000, 0.000000000000000000, 125.0000000000000000 ) ) ;
#4273 = LINE ( 'NONE', #5590, #1363 ) ;
#4274 = PRODUCT_DEFINITION ( 'UNKNOWN', '', #5302, #7282 ) ;
#4275 = DIRECTION ( 'NONE',  ( 0.000000000000000000, 1.224646799147353207E-16, 1.000000000000000000 ) ) ;
#4276 = DIRECTION ( 'NONE',  ( 0.000000000000000000, 0.000000000000000000, 1.000000000000000000 ) ) ;
#4277 = ORIENTED_EDGE ( 'NONE', *, *, #4340, .T. ) ;
#4278 = PRODUCT ( 'MAS-189', 'MAS-189', '', ( #1476 ) ) ;
#4279 = DIRECTION ( 'NONE',  ( -0.000000000000000000, 1.000000000000000000, 1.224646799147353207E-16 ) ) ;
#4280 = AXIS2_PLACEMENT_3D ( 'NONE', #5771, #2246, #1098 ) ;
#4281 = CARTESIAN_POINT ( 'NONE',  ( 0.6920835326022565237, 4.454600218803884459, -3.597382984111579862 ) ) ;
#4282 = VERTEX_POINT ( 'NONE', #2877 ) ;
#4283 =( LENGTH_UNIT ( ) NAMED_UNIT ( * ) SI_UNIT ( .MILLI., .METRE. ) );
#4284 = SURFACE_STYLE_FILL_AREA ( #1951 ) ;
#4285 = FACE_BOUND ( 'NONE', #247, .T. ) ;
#4286 = ORIENTED_EDGE ( 'NONE', *, *, #1176, .F. ) ;
#4287 = EDGE_CURVE ( 'NONE', #3428, #5461, #4051, .T. ) ;
#4288 = ORIENTED_EDGE ( 'NONE', *, *, #648, .F. ) ;
#4289 = CARTESIAN_POINT ( 'NONE',  ( 136.6666666666666288, -20.00000000000000000, 159.8500000000001080 ) ) ;
#4290 = DIRECTION ( 'NONE',  ( 1.000000000000000000, 0.000000000000000000, 0.000000000000000000 ) ) ;
#4291 =( LENGTH_UNIT ( ) NAMED_UNIT ( * ) SI_UNIT ( .MILLI., .METRE. ) );
#4292 = ORIENTED_EDGE ( 'NONE', *, *, #2403, .F. ) ;
#4293 = ADVANCED_FACE ( 'NONE', ( #4584 ), #1766, .F. ) ;
#4294 = CARTESIAN_POINT ( 'NONE',  ( -5.000000000000000888, -8.660254037844389075, 150.0000000000000000 ) ) ;
#4295 = CONTEXT_DEPENDENT_SHAPE_REPRESENTATION ( #5607, #5941 ) ;
#4296 = FACE_BOUND ( 'NONE', #6592, .T. ) ;
#4297 = FACE_BOUND ( 'NONE', #1877, .T. ) ;
#4298 = DIRECTION ( 'NONE',  ( 6.123233995736766036E-17, -1.000000000000000000, 0.000000000000000000 ) ) ;
#4299 = ORIENTED_EDGE ( 'NONE', *, *, #4756, .T. ) ;
#4300 = CARTESIAN_POINT ( 'NONE',  ( 405.0000000000000000, -8.660254037844389075, 140.0000000000000000 ) ) ;
#4301 = CIRCLE ( 'NONE', #2857, 2.649999999999985700 ) ;
#4302 = ORIENTED_EDGE ( 'NONE', *, *, #6923, .F. ) ;
#4303 = ORIENTED_EDGE ( 'NONE', *, *, #926, .F. ) ;
#4304 =( REPRESENTATION_RELATIONSHIP ('NONE','NONE', #5587, #1193 ) REPRESENTATION_RELATIONSHIP_WITH_TRANSFORMATION ( #3688 )SHAPE_REPRESENTATION_RELATIONSHIP( ) );
#4305 = EDGE_CURVE ( 'NONE', #1731, #5144, #4085, .T. ) ;
#4306 = DIRECTION ( 'NONE',  ( -0.000000000000000000, 1.000000000000000000, -0.000000000000000000 ) ) ;
#4307 = DIRECTION ( 'NONE',  ( 1.000000000000000000, 0.000000000000000000, 0.000000000000000000 ) ) ;
#4308 = DIRECTION ( 'NONE',  ( 0.000000000000000000, 1.000000000000000000, 0.000000000000000000 ) ) ;
#4309 = CARTESIAN_POINT ( 'NONE',  ( 219.9999999999999716, -20.00000000000000000, -162.5000000000000853 ) ) ;
#4310 = VECTOR ( 'NONE', #7129, 1000.000000000000000 ) ;
#4311 = DIRECTION ( 'NONE',  ( -1.000000000000000000, -0.000000000000000000, -0.000000000000000000 ) ) ;
#4312 = LINE ( 'NONE', #1355, #1007 ) ;
#4313 = PRODUCT_RELATED_PRODUCT_CATEGORY ( 'part', '', ( #2469 ) ) ;
#4314 = EDGE_LOOP ( 'NONE', ( #2882, #7064, #2424, #2228 ) ) ;
#4315 = VECTOR ( 'NONE', #4391, 1000.000000000000000 ) ;
#4316 = CARTESIAN_POINT ( 'NONE',  ( 124.9999999999999858, 8.660254037844390851, 145.0000000000000284 ) ) ;
#4317 = CARTESIAN_POINT ( 'NONE',  ( 0.000000000000000000, 0.000000000000000000, 11.75000000000000000 ) ) ;
#4318 = VERTEX_POINT ( 'NONE', #3447 ) ;
#4319 = DIRECTION ( 'NONE',  ( 0.000000000000000000, 0.000000000000000000, 1.000000000000000000 ) ) ;
#4320 = PRESENTATION_STYLE_ASSIGNMENT (( #2066 ) ) ;
#4321 = PLANE ( 'NONE',  #3988 ) ;
#4322 = CARTESIAN_POINT ( 'NONE',  ( 405.0000000000000000, 8.660254037844390851, 139.9990000000000236 ) ) ;
#4323 = ORIENTED_EDGE ( 'NONE', *, *, #1518, .T. ) ;
#4324 = DIRECTION ( 'NONE',  ( 0.000000000000000000, 0.000000000000000000, 1.000000000000000000 ) ) ;
#4325 = ORIENTED_EDGE ( 'NONE', *, *, #3569, .T. ) ;
#4326 = CARTESIAN_POINT ( 'NONE',  ( 325.0000000000000000, -8.660254037844389075, 139.9990000000000236 ) ) ;
#4327 = AXIS2_PLACEMENT_3D ( 'NONE', #1969, #6673, #376 ) ;
#4328 = EDGE_CURVE ( 'NONE', #3854, #1563, #3517, .T. ) ;
#4329 = CARTESIAN_POINT ( 'NONE',  ( -3.333333333333335258, 2.694301256218251783, -3.300726591567079815 ) ) ;
#4330 = DIRECTION ( 'NONE',  ( -0.000000000000000000, -0.000000000000000000, 1.000000000000000000 ) ) ;
#4331 = ORIENTED_EDGE ( 'NONE', *, *, #1364, .T. ) ;
#4332 = CARTESIAN_POINT ( 'NONE',  ( -20.63749999999999929, 0.000000000000000000, 0.000000000000000000 ) ) ;
#4333 = VECTOR ( 'NONE', #999, 1000.000000000000000 ) ;
#4334 = DIRECTION ( 'NONE',  ( -0.000000000000000000, 0.000000000000000000, 1.000000000000000000 ) ) ;
#4335 = DIRECTION ( 'NONE',  ( -0.000000000000000000, 0.000000000000000000, -1.000000000000000000 ) ) ;
#4336 = CARTESIAN_POINT ( 'NONE',  ( 200.0000000000000000, 0.000000000000000000, -123.0000000000000000 ) ) ;
#4337 = ORIENTED_EDGE ( 'NONE', *, *, #2728, .F. ) ;
#4338 = PLANE ( 'NONE',  #3375 ) ;
#4339 = PRODUCT_DEFINITION_SHAPE ( 'NONE', 'NONE',  #3195 ) ;
#4340 = EDGE_CURVE ( 'NONE', #3869, #7144, #2323, .T. ) ;
#4341 = AXIS2_PLACEMENT_3D ( 'NONE', #2089, #3278, #1574 ) ;
#4342 = AXIS2_PLACEMENT_3D ( 'NONE', #318, #7126, #4275 ) ;
#4343 = EDGE_CURVE ( 'NONE', #6959, #828, #2861, .T. ) ;
#4344 = AXIS2_PLACEMENT_3D ( 'NONE', #189, #4748, #7034 ) ;
#4345 = EDGE_LOOP ( 'NONE', ( #7014, #7201, #4459, #4759 ) ) ;
#4346 = ORIENTED_EDGE ( 'NONE', *, *, #3033, .T. ) ;
#4347 = DIRECTION ( 'NONE',  ( 0.000000000000000000, 0.8660254037844380415, -0.5000000000000012212 ) ) ;
#4348 = CARTESIAN_POINT ( 'NONE',  ( 2.836893136758676270, 3.208949435745843903, -3.505054077164911241 ) ) ;
#4349 = DIRECTION ( 'NONE',  ( 0.000000000000000000, -1.000000000000000000, 0.000000000000000000 ) ) ;
#4350 = DIRECTION ( 'NONE',  ( 1.000000000000000000, 0.000000000000000000, 0.000000000000000000 ) ) ;
#4351 =( GEOMETRIC_REPRESENTATION_CONTEXT ( 3 ) GLOBAL_UNCERTAINTY_ASSIGNED_CONTEXT ( ( #6763 ) ) GLOBAL_UNIT_ASSIGNED_CONTEXT ( ( #6290, #2920, #3422 ) ) REPRESENTATION_CONTEXT ( 'NONE', 'WORKASPACE' ) );
#4352 = CIRCLE ( 'NONE', #7217, 10.72499999999999964 ) ;
#4353 = DIRECTION ( 'NONE',  ( 1.000000000000000000, 0.000000000000000000, 0.000000000000000000 ) ) ;
#4354 = CARTESIAN_POINT ( 'NONE',  ( 470.0000000000000000, 0.000000000000000000, 145.0000000000000284 ) ) ;
#4355 = CARTESIAN_POINT ( 'NONE',  ( 0.000000000000000000, 0.000000000000000000, -4.000000000000000000 ) ) ;
#4356 = EDGE_CURVE ( 'NONE', #2028, #6041, #589, .T. ) ;
#4357 = ORIENTED_EDGE ( 'NONE', *, *, #7216, .F. ) ;
#4358 =( GEOMETRIC_REPRESENTATION_CONTEXT ( 3 ) GLOBAL_UNCERTAINTY_ASSIGNED_CONTEXT ( ( #4207 ) ) GLOBAL_UNIT_ASSIGNED_CONTEXT ( ( #2145, #7291, #5513 ) ) REPRESENTATION_CONTEXT ( 'NONE', 'WORKASPACE' ) );
#4359 = AXIS2_PLACEMENT_3D ( 'NONE', #2761, #6649, #2893 ) ;
#4360 = DIRECTION ( 'NONE',  ( 0.000000000000000000, -1.224646799147352468E-16, 1.000000000000000000 ) ) ;
#4361 = FACE_OUTER_BOUND ( 'NONE', #5097, .T. ) ;
#4362 = ORIENTED_EDGE ( 'NONE', *, *, #150, .F. ) ;
#4363 = CARTESIAN_POINT ( 'NONE',  ( 315.0000000000000568, -8.660254037844389075, 139.9990000000000236 ) ) ;
#4364 = VECTOR ( 'NONE', #3943, 1000.000000000000000 ) ;
#4365 = PLANE ( 'NONE',  #2778 ) ;
#4366 = AXIS2_PLACEMENT_3D ( 'NONE', #5922, #790, #2486 ) ;
#4367 = DIRECTION ( 'NONE',  ( -1.000000000000000000, -0.000000000000000000, -0.000000000000000000 ) ) ;
#4368 = ORIENTED_EDGE ( 'NONE', *, *, #5799, .F. ) ;
#4369 = CARTESIAN_POINT ( 'NONE',  ( 360.0000000000000000, 0.000000000000000000, 0.000000000000000000 ) ) ;
#4370 = AXIS2_PLACEMENT_3D ( 'NONE', #495, #1017, #3395 ) ;
#4371 = EDGE_LOOP ( 'NONE', ( #7139, #6887, #5252, #4855 ) ) ;
#4372 = AXIS2_PLACEMENT_3D ( 'NONE', #3516, #4624, #3446 ) ;
#4373 = CARTESIAN_POINT ( 'NONE',  ( -5.000000000000000888, 8.660254037844390851, 140.0000000000000000 ) ) ;
#4374 = ADVANCED_FACE ( 'NONE', ( #5118 ), #4519, .F. ) ;
#4375 = DIRECTION ( 'NONE',  ( -0.000000000000000000, 1.000000000000000000, -0.000000000000000000 ) ) ;
#4376 = FACE_OUTER_BOUND ( 'NONE', #1279, .T. ) ;
#4377 = AXIS2_PLACEMENT_3D ( 'NONE', #4644, #1758, #1786 ) ;
#4378 = EDGE_LOOP ( 'NONE', ( #3581, #5027, #4620, #404 ) ) ;
#4379 = DIRECTION ( 'NONE',  ( 0.000000000000000000, 1.000000000000000000, 0.000000000000000000 ) ) ;
#4380 = LINE ( 'NONE', #3192, #6484 ) ;
#4381 = CARTESIAN_POINT ( 'NONE',  ( 35.00000000000000000, 8.660254037844390851, 140.0000000000000000 ) ) ;
#4382 = VECTOR ( 'NONE', #6704, 1000.000000000000000 ) ;
#4383 = DIRECTION ( 'NONE',  ( 1.000000000000000000, 6.123233995736766036E-17, -6.123233995736764803E-17 ) ) ;
#4384 = B_SPLINE_CURVE_WITH_KNOTS ( 'NONE', 3,
 ( #614, #6911, #5175, #549, #5775, #4468 ),
 .UNSPECIFIED., .F., .F.,
 ( 4, 2, 4 ),
 ( 0.002452478801916361129, 0.003676905084148001344, 0.004901331366379641126 ),
 .UNSPECIFIED. ) ;
#4385 = EDGE_LOOP ( 'NONE', ( #4090, #5146, #4682, #1866, #6316 ) ) ;
#4386 = FACE_BOUND ( 'NONE', #147, .T. ) ;
#4387 = VERTEX_POINT ( 'NONE', #1213 ) ;
#4388 = AXIS2_PLACEMENT_3D ( 'NONE', #4805, #3796, #839 ) ;
#4389 = EDGE_CURVE ( 'NONE', #1598, #1884, #2285, .T. ) ;
#4390 = VERTEX_POINT ( 'NONE', #4026 ) ;
#4391 = DIRECTION ( 'NONE',  ( -0.000000000000000000, -0.000000000000000000, -1.000000000000000000 ) ) ;
#4392 = CARTESIAN_POINT ( 'NONE',  ( 235.0000000000000000, 8.660254037844390851, 139.9990000000000236 ) ) ;
#4393 = ITEM_DEFINED_TRANSFORMATION ( 'NONE', 'NONE', #5664,  #1963 ) ;
#4394 = CARTESIAN_POINT ( 'NONE',  ( 136.6666666666666288, -25.00000000000000000, -159.8500000000001080 ) ) ;
#4395 = DIRECTION ( 'NONE',  ( -0.000000000000000000, -1.000000000000000000, -0.000000000000000000 ) ) ;
#4396 = EDGE_CURVE ( 'NONE', #6971, #5618, #1182, .T. ) ;
#4397 = LINE ( 'NONE', #2699, #3387 ) ;
#4398 = DIRECTION ( 'NONE',  ( 0.000000000000000000, 0.000000000000000000, 1.000000000000000000 ) ) ;
#4399 = ORIENTED_EDGE ( 'NONE', *, *, #1919, .T. ) ;
#4400 = CARTESIAN_POINT ( 'NONE',  ( -20.63749999999999574, 1.524685264938454646E-15, 12.44999999999999929 ) ) ;
#4401 = DIRECTION ( 'NONE',  ( -1.000000000000000000, -0.000000000000000000, -0.000000000000000000 ) ) ;
#4402 = DIRECTION ( 'NONE',  ( -0.000000000000000000, -0.000000000000000000, 1.000000000000000000 ) ) ;
#4403 = CARTESIAN_POINT ( 'NONE',  ( 2.500000000000000000, 0.000000000000000000, 0.000000000000000000 ) ) ;
#4404 = EDGE_CURVE ( 'NONE', #7, #5278, #5745, .T. ) ;
#4405 = CARTESIAN_POINT ( 'NONE',  ( 1.411581201560190495E-15, 4.862606272033091592, -3.745885042887436622 ) ) ;
#4406 = CARTESIAN_POINT ( 'NONE',  ( 303.3333333333333144, -20.00000000000000000, 159.8500000000001080 ) ) ;
#4407 = EDGE_LOOP ( 'NONE', ( #2559, #5403, #3645, #4030 ) ) ;
#4408 = ORIENTED_EDGE ( 'NONE', *, *, #5176, .F. ) ;
#4409 = DIRECTION ( 'NONE',  ( 1.000000000000000000, 0.000000000000000000, 0.000000000000000000 ) ) ;
#4410 = ORIENTED_EDGE ( 'NONE', *, *, #5435, .F. ) ;
#4411 = EDGE_CURVE ( 'NONE', #709, #1728, #2664, .T. ) ;
#4412 = PRODUCT_DEFINITION_SHAPE ( 'NONE', 'NONE',  #213 ) ;
#4413 = DIRECTION ( 'NONE',  ( 1.000000000000000000, 0.000000000000000000, 0.000000000000000000 ) ) ;
#4414 = FACE_OUTER_BOUND ( 'NONE', #4976, .T. ) ;
#4415 = CARTESIAN_POINT ( 'NONE',  ( 136.6666666666666288, -20.00000000000000000, 159.8500000000001080 ) ) ;
#4416 = EDGE_LOOP ( 'NONE', ( #2008, #4331, #2349 ) ) ;
#4417 = B_SPLINE_CURVE_WITH_KNOTS ( 'NONE', 3,
 ( #436, #2698, #864, #7124, #3785, #1461, #7240, #3119 ),
 .UNSPECIFIED., .F., .F.,
 ( 4, 2, 2, 4 ),
 ( 0.005725059856848641743, 0.006314084072593626612, 0.006903108288338611481, 0.008081156719828581220 ),
 .UNSPECIFIED. ) ;
#4418 = DIRECTION ( 'NONE',  ( -0.000000000000000000, -0.000000000000000000, 1.000000000000000000 ) ) ;
#4419 = CARTESIAN_POINT ( 'NONE',  ( 13.50000000000000000, 0.000000000000000000, 121.0000000000000000 ) ) ;
#4420 = DIRECTION ( 'NONE',  ( 1.000000000000000000, 0.000000000000000000, 0.000000000000000000 ) ) ;
#4421 = ORIENTED_EDGE ( 'NONE', *, *, #419, .F. ) ;
#4422 = DIRECTION ( 'NONE',  ( 0.000000000000000000, -1.000000000000000000, 0.000000000000000000 ) ) ;
#4423 = ORIENTED_EDGE ( 'NONE', *, *, #2940, .F. ) ;
#4424 = ORIENTED_EDGE ( 'NONE', *, *, #1901, .T. ) ;
#4425 = DIRECTION ( 'NONE',  ( -0.000000000000000000, -0.000000000000000000, -1.000000000000000000 ) ) ;
#4426 = CARTESIAN_POINT ( 'NONE',  ( -4.211140560182196957, -2.431303136016552013, -3.745885042887436178 ) ) ;
#4427 = CARTESIAN_POINT ( 'NONE',  ( 2.059999999999998721, 0.000000000000000000, -0.3080913168122742518 ) ) ;
#4428 = DIRECTION ( 'NONE',  ( 0.000000000000000000, 0.000000000000000000, 1.000000000000000000 ) ) ;
#4429 = DIRECTION ( 'NONE',  ( 0.000000000000000000, 0.000000000000000000, 1.000000000000000000 ) ) ;
#4430 = FACE_OUTER_BOUND ( 'NONE', #4166, .T. ) ;
#4431 = ADVANCED_FACE ( 'NONE', ( #2816 ), #1147, .F. ) ;
#4432 = CIRCLE ( 'NONE', #3367, 2.649999999999985700 ) ;
#4433 = EDGE_LOOP ( 'NONE', ( #4672, #1132, #2293, #5210 ) ) ;
#4434 = CARTESIAN_POINT ( 'NONE',  ( 470.0000000000000000, 15.00000000000000000, 145.0000000000000284 ) ) ;
#4435 = DIRECTION ( 'NONE',  ( 0.000000000000000000, 0.000000000000000000, 1.000000000000000000 ) ) ;
#4436 = DIRECTION ( 'NONE',  ( 0.000000000000000000, 0.000000000000000000, 1.000000000000000000 ) ) ;
#4437 = DIRECTION ( 'NONE',  ( -1.000000000000000000, -0.000000000000000000, -0.000000000000000000 ) ) ;
#4438 = CARTESIAN_POINT ( 'NONE',  ( 1.567478505476134606E-15, 4.618802153517012066, -3.433295621305382905 ) ) ;
#4439 = VECTOR ( 'NONE', #919, 1000.000000000000000 ) ;
#4440 = VECTOR ( 'NONE', #1553, 1000.000000000000000 ) ;
#4441 = EDGE_CURVE ( 'NONE', #630, #6814, #6281, .T. ) ;
#4442 = ORIENTED_EDGE ( 'NONE', *, *, #2046, .F. ) ;
#4443 = EDGE_LOOP ( 'NONE', ( #2712, #3957, #366, #3603 ) ) ;
#4444 = DIRECTION ( 'NONE',  ( 1.000000000000000000, 0.000000000000000000, 0.000000000000000000 ) ) ;
#4445 = EDGE_LOOP ( 'NONE', ( #6634, #4535 ) ) ;
#4446 = CYLINDRICAL_SURFACE ( 'NONE', #5807, 13.50000000000000000 ) ;
#4447 = DIRECTION ( 'NONE',  ( -1.000000000000000000, 0.000000000000000000, -0.000000000000000000 ) ) ;
#4448 = LINE ( 'NONE', #1051, #7015 ) ;
#4449 = EDGE_CURVE ( 'NONE', #5855, #6847, #100, .T. ) ;
#4450 = EDGE_LOOP ( 'NONE', ( #641, #4259 ) ) ;
#4451 = CIRCLE ( 'NONE', #1804, 13.50000000000000000 ) ;
#4452 = FACE_OUTER_BOUND ( 'NONE', #3075, .T. ) ;
#4453 = CARTESIAN_POINT ( 'NONE',  ( 0.6448876103708359731, 4.246476118072354922, -0.2256878752776725616 ) ) ;
#4454 = AXIS2_PLACEMENT_3D ( 'NONE', #3928, #1711, #5728 ) ;
#4455 = DIRECTION ( 'NONE',  ( 0.000000000000000000, -1.000000000000000000, 0.000000000000000000 ) ) ;
#4456 = B_SPLINE_CURVE_WITH_KNOTS ( 'NONE', 3,
 ( #4426, #5068, #5236, #6119 ),
 .UNSPECIFIED., .F., .F.,
 ( 4, 4 ),
 ( 0.000000000000000000, 0.002452478801916376308 ),
 .UNSPECIFIED. ) ;
#4457 = CARTESIAN_POINT ( 'NONE',  ( 120.0000000000000000, 0.000000000000000000, 0.000000000000000000 ) ) ;
#4458 =( REPRESENTATION_RELATIONSHIP ('NONE','NONE', #5587, #951 ) REPRESENTATION_RELATIONSHIP_WITH_TRANSFORMATION ( #3504 )SHAPE_REPRESENTATION_RELATIONSHIP( ) );
#4459 = ORIENTED_EDGE ( 'NONE', *, *, #7193, .T. ) ;
#4460 = ORIENTED_EDGE ( 'NONE', *, *, #1373, .T. ) ;
#4461 = VERTEX_POINT ( 'NONE', #953 ) ;
#4462 = CARTESIAN_POINT ( 'NONE',  ( 395.0000000000000000, 8.660254037844390851, 139.9990000000000236 ) ) ;
#4463 = CARTESIAN_POINT ( 'NONE',  ( 45.00000000000000000, 8.660254037844390851, 145.0000000000000284 ) ) ;
#4464 = CARTESIAN_POINT ( 'NONE',  ( 4.000000000000000000, -2.309401076758516691, -0.4999999999999995559 ) ) ;
#4465 = LINE ( 'NONE', #1820, #1251 ) ;
#4466 = AXIS2_PLACEMENT_3D ( 'NONE', #3081, #3729, #3855 ) ;
#4467 = CARTESIAN_POINT ( 'NONE',  ( 303.3333333333333144, -20.00000000000000000, -159.8500000000001080 ) ) ;
#4468 = CARTESIAN_POINT ( 'NONE',  ( 4.211140560182196957, -2.431303136016555122, -3.745885042887436622 ) ) ;
#4469 = ORIENTED_EDGE ( 'NONE', *, *, #5094, .T. ) ;
#4470 = LINE ( 'NONE', #6769, #5872 ) ;
#4471 = DIRECTION ( 'NONE',  ( -1.000000000000000000, -0.000000000000000000, -0.000000000000000000 ) ) ;
#4472 = EDGE_LOOP ( 'NONE', ( #3624, #1704, #2460, #5883, #3042 ) ) ;
#4473 = ADVANCED_FACE ( 'NONE', ( #7248 ), #5472, .F. ) ;
#4474 = AXIS2_PLACEMENT_3D ( 'NONE', #1604, #3886, #6182 ) ;
#4475 = CARTESIAN_POINT ( 'NONE',  ( 4.999999999999999112, 0.000000000000000000, -140.0000000000000000 ) ) ;
#4476 = CARTESIAN_POINT ( 'NONE',  ( -1.799999999999996048, 1.249139735130300365E-15, 10.20000000000000107 ) ) ;
#4477 = CIRCLE ( 'NONE', #2189, 2.649999999999985700 ) ;
#4478 = VECTOR ( 'NONE', #4290, 1000.000000000000000 ) ;
#4479 = CARTESIAN_POINT ( 'NONE',  ( 470.0000000000000000, 15.00000000000000000, 140.0000000000000000 ) ) ;
#4480 = AXIS2_PLACEMENT_3D ( 'NONE', #1509, #3243, #1427 ) ;
#4481 = TOROIDAL_SURFACE ( 'NONE', #1721, 11.75000000000000000, 1.050000000000000266 ) ;
#4482 = ORIENTED_EDGE ( 'NONE', *, *, #6042, .F. ) ;
#4483 = VERTEX_POINT ( 'NONE', #2107 ) ;
#4484 = DIRECTION ( 'NONE',  ( 0.000000000000000000, 0.000000000000000000, -1.000000000000000000 ) ) ;
#4485 = VERTEX_POINT ( 'NONE', #6570 ) ;
#4486 = CIRCLE ( 'NONE', #6514, 2.500000000000001332 ) ;
#4487 =( GEOMETRIC_REPRESENTATION_CONTEXT ( 3 ) GLOBAL_UNCERTAINTY_ASSIGNED_CONTEXT ( ( #1584 ) ) GLOBAL_UNIT_ASSIGNED_CONTEXT ( ( #6374, #2417, #686 ) ) REPRESENTATION_CONTEXT ( 'NONE', 'WORKASPACE' ) );
#4488 = DIRECTION ( 'NONE',  ( -0.000000000000000000, -0.000000000000000000, 1.000000000000000000 ) ) ;
#4489 = ADVANCED_FACE ( 'NONE', ( #443 ), #323, .F. ) ;
#4490 = DIRECTION ( 'NONE',  ( 0.000000000000000000, 0.000000000000000000, -1.000000000000000000 ) ) ;
#4491 = AXIS2_PLACEMENT_3D ( 'NONE', #2797, #1056, #4566 ) ;
#4492 = VERTEX_POINT ( 'NONE', #5004 ) ;
#4493 = DIRECTION ( 'NONE',  ( 0.000000000000000000, 0.000000000000000000, -1.000000000000000000 ) ) ;
#4494 = DIRECTION ( 'NONE',  ( -1.000000000000000000, -0.000000000000000000, -0.000000000000000000 ) ) ;
#4495 = DIRECTION ( 'NONE',  ( -0.9396926207859138680, 0.000000000000000000, -0.3420201433256536139 ) ) ;
#4496 = EDGE_CURVE ( 'NONE', #4971, #3920, #1588, .T. ) ;
#4497 =( BOUNDED_SURFACE ( )  B_SPLINE_SURFACE ( 3, 2, ( 
 ( #7049, #4192, #273 ),
 ( #4160, #6451, #829 ),
 ( #1896, #6596, #3699 ),
 ( #7122, #752, #1310 ),
 ( #207, #4792, #3585 ),
 ( #5886, #1390, #2463 ) ),
 .UNSPECIFIED., .F., .F., .T. ) 
 B_SPLINE_SURFACE_WITH_KNOTS ( ( 4, 2, 4 ),
 ( 3, 3 ),
 ( 0.02032853247518126918, 0.02278863295364821906, 0.02524873343211516893 ),
 ( 0.000000000000000000, 1.000000000000000000 ),
 .UNSPECIFIED. ) 
 GEOMETRIC_REPRESENTATION_ITEM ( )  RATIONAL_B_SPLINE_SURFACE ( (
 ( 1.000000000000000000, 0.8047781615896838492, 1.000000000000000000),
 ( 1.000000000000000000, 0.8123767586288186404, 1.000000000000000000),
 ( 1.000000000000000000, 0.8190662415565814758, 1.000000000000000000),
 ( 1.000000000000000000, 0.8192361015667604107, 1.000000000000000000),
 ( 1.000000000000000000, 0.8126135807104967190, 1.000000000000000000),
 ( 1.000000000000000000, 0.8047712338318580017, 1.000000000000000000) ) ) 
 REPRESENTATION_ITEM ( '' )  SURFACE ( )  );
#4498 = AXIS2_PLACEMENT_3D ( 'NONE', #2785, #3385, #2715 ) ;
#4499 = DIRECTION ( 'NONE',  ( -1.000000000000000000, -6.123233995736766036E-17, -6.123233995736764803E-17 ) ) ;
#4500 = ORIENTED_EDGE ( 'NONE', *, *, #4854, .F. ) ;
#4501 = CARTESIAN_POINT ( 'NONE',  ( 325.0000000000000000, 8.660254037844390851, 139.9990000000000236 ) ) ;
#4502 = EDGE_CURVE ( 'NONE', #5646, #3234, #137, .T. ) ;
#4503 = ORIENTED_EDGE ( 'NONE', *, *, #1197, .F. ) ;
#4504 = EDGE_LOOP ( 'NONE', ( #2015, #2509, #5453, #5774 ) ) ;
#4505 = CARTESIAN_POINT ( 'NONE',  ( 4.211140560182196957, 2.431303136016536470, -3.745885042887433514 ) ) ;
#4506 = CIRCLE ( 'NONE', #2096, 0.2000000000000022593 ) ;
#4507 = DIRECTION ( 'NONE',  ( 1.000000000000000000, 0.000000000000000000, 0.000000000000000000 ) ) ;
#4508 = ITEM_DEFINED_TRANSFORMATION ( 'NONE', 'NONE', #6978,  #1963 ) ;
#4509 = CARTESIAN_POINT ( 'NONE',  ( -5.000000000000000888, -8.660254037844389075, -150.0000000000000000 ) ) ;
#4510 = DIRECTION ( 'NONE',  ( 1.000000000000000000, 0.000000000000000000, 0.000000000000000000 ) ) ;
#4511 =( REPRESENTATION_RELATIONSHIP ('NONE','NONE', #5587, #4771 ) REPRESENTATION_RELATIONSHIP_WITH_TRANSFORMATION ( #1290 )SHAPE_REPRESENTATION_RELATIONSHIP( ) );
#4512 = CYLINDRICAL_SURFACE ( 'NONE', #1481, 2.649999999999985700 ) ;
#4513 = LINE ( 'NONE', #6765, #6985 ) ;
#4514 = AXIS2_PLACEMENT_3D ( 'NONE', #7220, #1412, #3185 ) ;
#4515 = ORIENTED_EDGE ( 'NONE', *, *, #5900, .F. ) ;
#4516 = EDGE_CURVE ( 'NONE', #5828, #841, #358, .T. ) ;
#4517 = DIRECTION ( 'NONE',  ( 1.000000000000000000, 0.000000000000000000, -0.000000000000000000 ) ) ;
#4518 = DIRECTION ( 'NONE',  ( -0.000000000000000000, 1.000000000000000000, -0.000000000000000000 ) ) ;
#4519 = PLANE ( 'NONE',  #3836 ) ;
#4520 = CARTESIAN_POINT ( 'NONE',  ( 0.000000000000000000, 0.000000000000000000, 145.0000000000000284 ) ) ;
#4521 = DIRECTION ( 'NONE',  ( 0.000000000000000000, -0.8660254037844390407, -0.4999999999999994449 ) ) ;
#4522=STYLED_ITEM('',(#7418),#5676);
#4523 = ORIENTED_EDGE ( 'NONE', *, *, #1151, .T. ) ;
#4524 = ORIENTED_EDGE ( 'NONE', *, *, #4247, .T. ) ;
#4525 = DIRECTION ( 'NONE',  ( 0.000000000000000000, 0.000000000000000000, 1.000000000000000000 ) ) ;
#4526 = EDGE_LOOP ( 'NONE', ( #4591, #550, #5369, #226 ) ) ;
#4527 = CARTESIAN_POINT ( 'NONE',  ( 315.0000000000000568, -8.660254037844389075, 139.9990000000000236 ) ) ;
#4528 = CARTESIAN_POINT ( 'NONE',  ( 3.511755186886750923, -2.826662030176382956, -3.597382984111582083 ) ) ;
#4529 = EDGE_CURVE ( 'NONE', #6988, #6671, #1516, .T. ) ;
#4530 = VERTEX_POINT ( 'NONE', #4876 ) ;
#4531 = CARTESIAN_POINT ( 'NONE',  ( 53.33333333333330017, -20.00000000000000000, -162.5000000000000853 ) ) ;
#4532 = DIRECTION ( 'NONE',  ( -1.000000000000000000, -0.000000000000000000, -0.000000000000000000 ) ) ;
#4533 = DIRECTION ( 'NONE',  ( -0.000000000000000000, -0.000000000000000000, 1.000000000000000000 ) ) ;
#4534 = DIRECTION ( 'NONE',  ( 0.000000000000000000, 0.000000000000000000, -1.000000000000000000 ) ) ;
#4535 = ORIENTED_EDGE ( 'NONE', *, *, #3890, .F. ) ;
#4536 = LINE ( 'NONE', #6827, #4757 ) ;
#4537 = EDGE_CURVE ( 'NONE', #2492, #5914, #871, .T. ) ;
#4538 = ORIENTED_EDGE ( 'NONE', *, *, #2365, .F. ) ;
#4539 = DIRECTION ( 'NONE',  ( 0.000000000000000000, 0.000000000000000000, 1.000000000000000000 ) ) ;
#4540 = LINE ( 'NONE', #1232, #2221 ) ;
#4541 = DIRECTION ( 'NONE',  ( -1.000000000000000000, 0.000000000000000000, 0.000000000000000000 ) ) ;
#4542 = LINE ( 'NONE', #6760, #6891 ) ;
#4543 = ORIENTED_EDGE ( 'NONE', *, *, #6956, .T. ) ;
#4544 = CARTESIAN_POINT ( 'NONE',  ( -1.800000000000002931, 1.653273178848927064E-15, 13.50000000000000355 ) ) ;
#4545 = ADVANCED_FACE ( 'NONE', ( #397 ), #4963, .T. ) ;
#4546 = ORIENTED_EDGE ( 'NONE', *, *, #3186, .T. ) ;
#4547 = FACE_OUTER_BOUND ( 'NONE', #501, .T. ) ;
#4548 = DIRECTION ( 'NONE',  ( 0.000000000000000000, 0.000000000000000000, -1.000000000000000000 ) ) ;
#4549 = CARTESIAN_POINT ( 'NONE',  ( 275.0000000000000000, 8.660254037844390851, 139.9990000000000236 ) ) ;
#4550 = DIRECTION ( 'NONE',  ( 1.000000000000000000, 0.000000000000000000, 0.000000000000000000 ) ) ;
#4551 = DIRECTION ( 'NONE',  ( 0.000000000000000000, 0.000000000000000000, 1.000000000000000000 ) ) ;
#4552 = PRODUCT_RELATED_PRODUCT_CATEGORY ( 'part', '', ( #4155 ) ) ;
#4553 = ORIENTED_EDGE ( 'NONE', *, *, #3120, .T. ) ;
#4554 = ORIENTED_EDGE ( 'NONE', *, *, #6825, .T. ) ;
#4555 = CIRCLE ( 'NONE', #3958, 10.00000000000000000 ) ;
#4556 = PRODUCT_CONTEXT ( 'NONE', #5129, 'mechanical' ) ;
#4557 = VERTEX_POINT ( 'NONE', #7203 ) ;
#4558 = PRODUCT_DEFINITION_SHAPE ( 'NONE', 'NONE',  #7386 ) ;
#4559 = PLANE ( 'NONE',  #4498 ) ;
#4560 = VECTOR ( 'NONE', #3653, 1000.000000000000000 ) ;
#4561 = LINE ( 'NONE', #1083, #3774 ) ;
#4562 = ORIENTED_EDGE ( 'NONE', *, *, #648, .T. ) ;
#4563 = VECTOR ( 'NONE', #5355, 1000.000000000000000 ) ;
#4564 = DIRECTION ( 'NONE',  ( 0.000000000000000000, 0.000000000000000000, -1.000000000000000000 ) ) ;
#4565 = EDGE_CURVE ( 'NONE', #2874, #5656, #2580, .T. ) ;
#4566 = DIRECTION ( 'NONE',  ( 0.000000000000000000, 0.000000000000000000, 1.000000000000000000 ) ) ;
#4567 = CARTESIAN_POINT ( 'NONE',  ( 80.00000000000000000, 0.000000000000000000, 0.000000000000000000 ) ) ;
#4568 = ORIENTED_EDGE ( 'NONE', *, *, #6276, .F. ) ;
#4569 = DIRECTION ( 'NONE',  ( 1.000000000000000000, 0.000000000000000000, 0.000000000000000000 ) ) ;
#4570 = ORIENTED_EDGE ( 'NONE', *, *, #6789, .T. ) ;
#4571 = CARTESIAN_POINT ( 'NONE',  ( 4.197393957002303999, 0.8151795401431359833, -3.503767560748935139 ) ) ;
#4572 = FACE_OUTER_BOUND ( 'NONE', #4133, .T. ) ;
#4573 = ITEM_DEFINED_TRANSFORMATION ( 'NONE', 'NONE', #6996,  #1963 ) ;
#4574 = CARTESIAN_POINT ( 'NONE',  ( -5.000000000000000888, 8.660254037844390851, 140.0000000000000000 ) ) ;
#4575 = DIRECTION ( 'NONE',  ( 0.000000000000000000, 0.000000000000000000, 1.000000000000000000 ) ) ;
#4576 = EDGE_CURVE ( 'NONE', #7309, #4282, #5436, .T. ) ;
#4577 = AXIS2_PLACEMENT_3D ( 'NONE', #4161, #3586, #753 ) ;
#4578 = ORIENTED_EDGE ( 'NONE', *, *, #2586, .T. ) ;
#4579 = FACE_OUTER_BOUND ( 'NONE', #4735, .T. ) ;
#4580 = EDGE_CURVE ( 'NONE', #1932, #3114, #1938, .T. ) ;
#4581 = ORIENTED_EDGE ( 'NONE', *, *, #4734, .T. ) ;
#4582 = DIRECTION ( 'NONE',  ( 0.000000000000000000, 1.000000000000000000, 0.000000000000000000 ) ) ;
#4583 = DIRECTION ( 'NONE',  ( 0.000000000000000000, -0.4999999999999992784, 0.8660254037844389297 ) ) ;
#4584 = FACE_OUTER_BOUND ( 'NONE', #3272, .T. ) ;
#4585 = CARTESIAN_POINT ( 'NONE',  ( 435.0000000000000568, 8.660254037844390851, 145.0000000000000284 ) ) ;
#4586 = AXIS2_PLACEMENT_3D ( 'NONE', #2129, #4422, #4824 ) ;
#4587 = ADVANCED_FACE ( 'NONE', ( #3132, #7164 ), #4839, .T. ) ;
#4588 = ORIENTED_EDGE ( 'NONE', *, *, #6376, .T. ) ;
#4589 = AXIS2_PLACEMENT_3D ( 'NONE', #2431, #5970, #3588 ) ;
#4590 = AXIS2_PLACEMENT_3D ( 'NONE', #6700, #6737, #2184 ) ;
#4591 = ORIENTED_EDGE ( 'NONE', *, *, #4496, .T. ) ;
#4592 = CIRCLE ( 'NONE', #2301, 4.000000000000000000 ) ;
#4593 = ORIENTED_EDGE ( 'NONE', *, *, #4803, .T. ) ;
#4594 =( NAMED_UNIT ( * ) SI_UNIT ( $, .STERADIAN. ) SOLID_ANGLE_UNIT ( ) );
#4595 = AXIS2_PLACEMENT_3D ( 'NONE', #3383, #1703, #594 ) ;
#4596 = AXIS2_PLACEMENT_3D ( 'NONE', #6224, #535, #5106 ) ;
#4597 = CIRCLE ( 'NONE', #6629, 10.20000000000000107 ) ;
#4598 = DIRECTION ( 'NONE',  ( -0.000000000000000000, 1.000000000000000000, -0.000000000000000000 ) ) ;
#4599 = VERTEX_POINT ( 'NONE', #4316 ) ;
#4600 =( REPRESENTATION_RELATIONSHIP ('NONE','NONE', #5587, #5294 ) REPRESENTATION_RELATIONSHIP_WITH_TRANSFORMATION ( #785 )SHAPE_REPRESENTATION_RELATIONSHIP( ) );
#4601 = CIRCLE ( 'NONE', #296, 4.000000000000000000 ) ;
#4602 = EDGE_CURVE ( 'NONE', #1207, #3032, #2141, .T. ) ;
#4603 = DIRECTION ( 'NONE',  ( -0.000000000000000000, 1.000000000000000000, -0.000000000000000000 ) ) ;
#4604 = DIRECTION ( 'NONE',  ( 0.000000000000000000, -1.000000000000000000, 1.287488025362403787E-15 ) ) ;
#4605 = DIRECTION ( 'NONE',  ( 6.123233995736766036E-17, -1.000000000000000000, 0.000000000000000000 ) ) ;
#4606 = ORIENTED_EDGE ( 'NONE', *, *, #418, .T. ) ;
#4607 = CIRCLE ( 'NONE', #6292, 13.50000000000000000 ) ;
#4608 = FACE_OUTER_BOUND ( 'NONE', #454, .T. ) ;
#4609 = AXIS2_PLACEMENT_3D ( 'NONE', #5255, #5790, #3927 ) ;
#4610 = ORIENTED_EDGE ( 'NONE', *, *, #6234, .F. ) ;
#4611 = CARTESIAN_POINT ( 'NONE',  ( 0.000000000000000000, 0.000000000000000000, 121.0000000000000000 ) ) ;
#4612 = CARTESIAN_POINT ( 'NONE',  ( 219.9999999999999716, -15.00000000000000000, 162.5000000000000853 ) ) ;
#4613 = ITEM_DEFINED_TRANSFORMATION ( 'NONE', 'NONE', #1123,  #1963 ) ;
#4614 = LINE ( 'NONE', #6312, #277 ) ;
#4615 = LINE ( 'NONE', #4044, #774 ) ;
#4616 = AXIS2_PLACEMENT_3D ( 'NONE', #655, #6974, #2913 ) ;
#4617 = ORIENTED_EDGE ( 'NONE', *, *, #4152, .F. ) ;
#4618 = DIRECTION ( 'NONE',  ( 1.000000000000000000, 0.000000000000000000, 0.000000000000000000 ) ) ;
#4619 = EDGE_CURVE ( 'NONE', #5646, #3709, #4910, .T. ) ;
#4620 = ORIENTED_EDGE ( 'NONE', *, *, #5376, .T. ) ;
#4621 = PRODUCT_DEFINITION_SHAPE ( 'NONE', 'NONE',  #7405 ) ;
#4622 = EDGE_CURVE ( 'NONE', #3461, #5483, #1985, .T. ) ;
#4623 = CARTESIAN_POINT ( 'NONE',  ( 1.317756351988342622, -3.857995168970215438, -0.04852650426602527628 ) ) ;
#4624 = DIRECTION ( 'NONE',  ( 0.000000000000000000, 1.000000000000000000, 0.000000000000000000 ) ) ;
#4625 = CARTESIAN_POINT ( 'NONE',  ( 4.000000000000003553, -2.309401076758513138, -3.504271511726786859 ) ) ;
#4626 = AXIS2_PLACEMENT_3D ( 'NONE', #5127, #7300, #39 ) ;
#4627 = CARTESIAN_POINT ( 'NONE',  ( 235.0000000000000000, 8.660254037844390851, 140.0000000000000000 ) ) ;
#4628 = ORIENTED_EDGE ( 'NONE', *, *, #6098, .F. ) ;
#4629 = ADVANCED_FACE ( 'NONE', ( #3913 ), #6843, .T. ) ;
#4630 = DIRECTION ( 'NONE',  ( 0.000000000000000000, 0.000000000000000000, 1.000000000000000000 ) ) ;
#4631 = ORIENTED_EDGE ( 'NONE', *, *, #2721, .F. ) ;
#4632 = CIRCLE ( 'NONE', #1396, 2.649999999999985700 ) ;
#4633 = DIRECTION ( 'NONE',  ( 0.000000000000000000, -0.000000000000000000, -1.000000000000000000 ) ) ;
#4634 = VERTEX_POINT ( 'NONE', #2217 ) ;
#4635 = ADVANCED_FACE ( 'NONE', ( #2844, #6237, #3445, #3414, #479, #5743 ), #6914, .F. ) ;
#4636 = DIRECTION ( 'NONE',  ( 0.000000000000000000, 0.000000000000000000, 1.000000000000000000 ) ) ;
#4637 = LINE ( 'NONE', #2958, #3888 ) ;
#4638 = EDGE_LOOP ( 'NONE', ( #2093, #7180, #1431, #4173 ) ) ;
#4639 = FILL_AREA_STYLE_COLOUR ( '', #1858 ) ;
#4640 = ORIENTED_EDGE ( 'NONE', *, *, #5444, .F. ) ;
#4641 = DIRECTION ( 'NONE',  ( 0.000000000000000000, 1.000000000000000000, 0.000000000000000000 ) ) ;
#4642 = ORIENTED_EDGE ( 'NONE', *, *, #976, .F. ) ;
#4643 = CARTESIAN_POINT ( 'NONE',  ( -1.999999999999998668, 1.249139735130300365E-15, 10.20000000000000107 ) ) ;
#4644 = CARTESIAN_POINT ( 'NONE',  ( -5.000000000000000888, 8.660254037844390851, 139.9990000000000236 ) ) ;
#4645 = DIRECTION ( 'NONE',  ( 0.000000000000000000, -1.000000000000000000, 0.000000000000000000 ) ) ;
#4646 = DIRECTION ( 'NONE',  ( -1.000000000000000000, -0.000000000000000000, -0.000000000000000000 ) ) ;
#4647 = ORIENTED_EDGE ( 'NONE', *, *, #7052, .F. ) ;
#4648 = CARTESIAN_POINT ( 'NONE',  ( 0.000000000000000000, 0.000000000000000000, -0.3080913168122742518 ) ) ;
#4649 = ORIENTED_EDGE ( 'NONE', *, *, #4619, .F. ) ;
#4650 = DIRECTION ( 'NONE',  ( -0.000000000000000000, 1.000000000000000000, -0.000000000000000000 ) ) ;
#4651 = CARTESIAN_POINT ( 'NONE',  ( 4.211140560182196957, -2.431303136016555122, -3.745885042887436622 ) ) ;
#4652 = CARTESIAN_POINT ( 'NONE',  ( 219.9999999999999716, -14.99999999999999822, 162.5000000000000853 ) ) ;
#4653 = FACE_BOUND ( 'NONE', #372, .T. ) ;
#4654 = ADVANCED_FACE ( 'NONE', ( #7322 ), #4038, .T. ) ;
#4655 = FACE_OUTER_BOUND ( 'NONE', #4526, .T. ) ;
#4656 = ORIENTED_EDGE ( 'NONE', *, *, #5314, .T. ) ;
#4657 = VERTEX_POINT ( 'NONE', #2813 ) ;
#4658 = CARTESIAN_POINT ( 'NONE',  ( 0.000000000000000000, 0.000000000000000000, -25.03750572909317285 ) ) ;
#4659 = ORIENTED_EDGE ( 'NONE', *, *, #2068, .F. ) ;
#4660 = SURFACE_STYLE_USAGE ( .BOTH. , #5792 ) ;
#4661 = ADVANCED_FACE ( 'NONE', ( #2875 ), #4049, .F. ) ;
#4662 = CARTESIAN_POINT ( 'NONE',  ( -4.000000000000000000, 0.8576368993457507139, -3.433240632782198709 ) ) ;
#4663 = ADVANCED_FACE ( 'NONE', ( #4547 ), #2250, .F. ) ;
#4664 = ORIENTED_EDGE ( 'NONE', *, *, #2459, .F. ) ;
#4665 = SURFACE_STYLE_USAGE ( .BOTH. , #2367 ) ;
#4666 = DIRECTION ( 'NONE',  ( 1.000000000000000000, 0.000000000000000000, 0.000000000000000000 ) ) ;
#4667 = AXIS2_PLACEMENT_3D ( 'NONE', #2552, #6507, #3915 ) ;
#4668 = ADVANCED_FACE ( 'NONE', ( #62 ), #346, .F. ) ;
#4669 = ORIENTED_EDGE ( 'NONE', *, *, #4622, .T. ) ;
#4670 = LINE ( 'NONE', #7001, #4560 ) ;
#4671 = CIRCLE ( 'NONE', #6355, 0.2000000000000022593 ) ;
#4672 = ORIENTED_EDGE ( 'NONE', *, *, #1060, .F. ) ;
#4673 = AXIS2_PLACEMENT_3D ( 'NONE', #5670, #6207, #3371 ) ;
#4674 = ADVANCED_FACE ( 'NONE', ( #5077 ), #5039, .F. ) ;
#4675 = DIRECTION ( 'NONE',  ( -1.000000000000000000, -0.000000000000000000, -0.000000000000000000 ) ) ;
#4676 = CARTESIAN_POINT ( 'NONE',  ( 219.9999999999999716, -25.00000000000000000, 165.1500000000000625 ) ) ;
#4677 = CARTESIAN_POINT ( 'NONE',  ( 1.243802165048773611, -3.900692638707475624, -3.223146290109810241 ) ) ;
#4678 = LINE ( 'NONE', #5957, #4117 ) ;
#4679 = ORIENTED_EDGE ( 'NONE', *, *, #6613, .T. ) ;
#4680 = CARTESIAN_POINT ( 'NONE',  ( 245.0000000000000000, -8.660254037844389075, 145.0000000000000284 ) ) ;
#4681 = UNCERTAINTY_MEASURE_WITH_UNIT (LENGTH_MEASURE( 1.000000000000000082E-05 ), #3420, 'distance_accuracy_value', 'NONE');
#4682 = ORIENTED_EDGE ( 'NONE', *, *, #70, .F. ) ;
#4683 = EDGE_LOOP ( 'NONE', ( #3115, #4866, #4679, #6439, #6225, #1327, #384, #7301 ) ) ;
#4684 = CARTESIAN_POINT ( 'NONE',  ( -2.000000000000001776, 0.000000000000000000, 0.000000000000000000 ) ) ;
#4685 = PLANE ( 'NONE',  #6412 ) ;
#4686 = CARTESIAN_POINT ( 'NONE',  ( 84.99999999999998579, 8.660254037844390851, 140.0000000000000000 ) ) ;
#4687 = DIRECTION ( 'NONE',  ( 1.000000000000000000, 0.000000000000000000, 0.000000000000000000 ) ) ;
#4688 = AXIS2_PLACEMENT_3D ( 'NONE', #2521, #786, #5842 ) ;
#4689 = VECTOR ( 'NONE', #4261, 1000.000000000000000 ) ;
#4690 = CARTESIAN_POINT ( 'NONE',  ( 136.6666666666666288, -25.00000000000000000, 165.1500000000000625 ) ) ;
#4691 =( REPRESENTATION_RELATIONSHIP ('NONE','NONE', #5587, #5294 ) REPRESENTATION_RELATIONSHIP_WITH_TRANSFORMATION ( #3941 )SHAPE_REPRESENTATION_RELATIONSHIP( ) );
#4692 = VERTEX_POINT ( 'NONE', #2175 ) ;
#4693 = ORIENTED_EDGE ( 'NONE', *, *, #2955, .T. ) ;
#4694 = EDGE_CURVE ( 'NONE', #84, #1308, #4470, .T. ) ;
#4695 = FACE_OUTER_BOUND ( 'NONE', #498, .T. ) ;
#4696 = VERTEX_POINT ( 'NONE', #3983 ) ;
#4697 = CIRCLE ( 'NONE', #755, 10.00000000000000000 ) ;
#4698 =( GEOMETRIC_REPRESENTATION_CONTEXT ( 3 ) GLOBAL_UNCERTAINTY_ASSIGNED_CONTEXT ( ( #2171 ) ) GLOBAL_UNIT_ASSIGNED_CONTEXT ( ( #3079, #4118, #265 ) ) REPRESENTATION_CONTEXT ( 'NONE', 'WORKASPACE' ) );
#4699 = CARTESIAN_POINT ( 'NONE',  ( -4.000000000000000000, -0.8232339106130515116, -3.430630286862743183 ) ) ;
#4700 = VECTOR ( 'NONE', #6548, 1000.000000000000000 ) ;
#4701 = ORIENTED_EDGE ( 'NONE', *, *, #5619, .F. ) ;
#4702 = ADVANCED_FACE ( 'NONE', ( #553 ), #6806, .F. ) ;
#4703 = EDGE_CURVE ( 'NONE', #5828, #380, #507, .T. ) ;
#4704 = VECTOR ( 'NONE', #1676, 1000.000000000000000 ) ;
#4705 = LINE ( 'NONE', #391, #3992 ) ;
#4706 = CARTESIAN_POINT ( 'NONE',  ( 219.9999999999999716, -20.00000000000000000, 159.8500000000001080 ) ) ;
#4707 = CIRCLE ( 'NONE', #2891, 2.649999999999985700 ) ;
#4708 = AXIS2_PLACEMENT_3D ( 'NONE', #4648, #2489, #200 ) ;
#4709 = CARTESIAN_POINT ( 'NONE',  ( 0.000000000000000000, 0.000000000000000000, 121.0000000000000000 ) ) ;
#4710 = CARTESIAN_POINT ( 'NONE',  ( 2.500000000000000888, 3.061616997868384127E-16, -4.974599999999998801 ) ) ;
#4711 = VECTOR ( 'NONE', #2817, 1000.000000000000000 ) ;
#4712 = EDGE_LOOP ( 'NONE', ( #5978, #55 ) ) ;
#4713 =( GEOMETRIC_REPRESENTATION_CONTEXT ( 3 ) GLOBAL_UNCERTAINTY_ASSIGNED_CONTEXT ( ( #7062 ) ) GLOBAL_UNIT_ASSIGNED_CONTEXT ( ( #4138, #6464, #4594 ) ) REPRESENTATION_CONTEXT ( 'NONE', 'WORKASPACE' ) );
#4714 = EDGE_CURVE ( 'NONE', #2565, #4184, #6600, .T. ) ;
#4715 = DIRECTION ( 'NONE',  ( -0.000000000000000000, 1.000000000000000000, -0.000000000000000000 ) ) ;
#4716 = DIRECTION ( 'NONE',  ( 0.000000000000000000, 0.000000000000000000, -1.000000000000000000 ) ) ;
#4717 = CARTESIAN_POINT ( 'NONE',  ( 0.5469614295415388128, -4.303013824935362663, -3.535263753543555598 ) ) ;
#4718 = DIRECTION ( 'NONE',  ( 0.000000000000000000, 0.000000000000000000, -1.000000000000000000 ) ) ;
#4719 = AXIS2_PLACEMENT_3D ( 'NONE', #2839, #1726, #1620 ) ;
#4720 = EDGE_LOOP ( 'NONE', ( #2122, #5749, #1114, #4807 ) ) ;
#4721 = EDGE_CURVE ( 'NONE', #7308, #2488, #1210, .T. ) ;
#4722 = CARTESIAN_POINT ( 'NONE',  ( 2.500000000000000000, 2.357898499370433054, -1.951563910473907981E-15 ) ) ;
#4723 = ORIENTED_EDGE ( 'NONE', *, *, #3551, .F. ) ;
#4724 = VECTOR ( 'NONE', #5523, 1000.000000000000000 ) ;
#4725 = ORIENTED_EDGE ( 'NONE', *, *, #7080, .T. ) ;
#4726 = ADVANCED_FACE ( 'NONE', ( #5817 ), #5215, .F. ) ;
#4727 = CARTESIAN_POINT ( 'NONE',  ( 4.000000000000000000, -1.084202172485504434E-14, -3.142992957459231906 ) ) ;
#4728 = VECTOR ( 'NONE', #3335, 1000.000000000000000 ) ;
#4729 = CARTESIAN_POINT ( 'NONE',  ( -1.360585162435467455, 4.061296242128285883, -3.505054077164959203 ) ) ;
#4730 = LINE ( 'NONE', #4128, #3250 ) ;
#4731 = DIRECTION ( 'NONE',  ( 1.000000000000000000, 0.000000000000000000, 0.000000000000000000 ) ) ;
#4732 = CARTESIAN_POINT ( 'NONE',  ( -2.344047193898593395, -3.265465875126480455, -1.054683074273691752E-14 ) ) ;
#4733 = CIRCLE ( 'NONE', #5446, 2.649999999999985700 ) ;
#4734 = EDGE_CURVE ( 'NONE', #2249, #7192, #1792, .T. ) ;
#4735 = EDGE_LOOP ( 'NONE', ( #1803, #219, #3776, #3728 ) ) ;
#4736 = EDGE_LOOP ( 'NONE', ( #1586, #6943, #4368, #1642 ) ) ;
#4737 = ITEM_DEFINED_TRANSFORMATION ( 'NONE', 'NONE', #2203,  #1963 ) ;
#4738 = CARTESIAN_POINT ( 'NONE',  ( 2.500000000000000000, 0.000000000000000000, 0.000000000000000000 ) ) ;
#4739 = ORIENTED_EDGE ( 'NONE', *, *, #7160, .F. ) ;
#4740 = PRODUCT_DEFINITION_SHAPE ( 'NONE', 'NONE',  #7376 ) ;
#4741 =( LENGTH_UNIT ( ) NAMED_UNIT ( * ) SI_UNIT ( .MILLI., .METRE. ) );
#4742 = FACE_OUTER_BOUND ( 'NONE', #6059, .T. ) ;
#4743 = UNCERTAINTY_MEASURE_WITH_UNIT (LENGTH_MEASURE( 1.000000000000000082E-05 ), #2506, 'distance_accuracy_value', 'NONE');
#4744 = CIRCLE ( 'NONE', #2453, 5.384454397937118664 ) ;
#4745 = ORIENTED_EDGE ( 'NONE', *, *, #2507, .T. ) ;
#4746 = PLANE ( 'NONE',  #1375 ) ;
#4747 = ADVANCED_FACE ( 'NONE', ( #7083 ), #6590, .T. ) ;
#4748 = DIRECTION ( 'NONE',  ( -1.000000000000000000, 0.000000000000000000, 0.000000000000000000 ) ) ;
#4749 =( LENGTH_UNIT ( ) NAMED_UNIT ( * ) SI_UNIT ( .MILLI., .METRE. ) );
#4750 = ORIENTED_EDGE ( 'NONE', *, *, #6168, .T. ) ;
#4751 = DIRECTION ( 'NONE',  ( 1.000000000000000000, 0.000000000000000000, 0.000000000000000000 ) ) ;
#4752 = DIRECTION ( 'NONE',  ( 1.000000000000000000, 0.000000000000000000, 0.000000000000000000 ) ) ;
#4753 = CARTESIAN_POINT ( 'NONE',  ( -31.74999999999995737, 0.000000000000000000, 0.000000000000000000 ) ) ;
#4754 = ORIENTED_EDGE ( 'NONE', *, *, #4576, .F. ) ;
#4755 = CARTESIAN_POINT ( 'NONE',  ( -2.804994570502171047, -3.229033611042465335, -3.526374918436838701 ) ) ;
#4756 = EDGE_CURVE ( 'NONE', #5845, #5499, #1346, .T. ) ;
#4757 = VECTOR ( 'NONE', #1682, 1000.000000000000000 ) ;
#4758 = VERTEX_POINT ( 'NONE', #1831 ) ;
#4759 = ORIENTED_EDGE ( 'NONE', *, *, #6416, .F. ) ;
#4760 = DIRECTION ( 'NONE',  ( 0.000000000000000000, 0.000000000000000000, -1.000000000000000000 ) ) ;
#4761 = DIRECTION ( 'NONE',  ( 0.000000000000000000, -1.000000000000000000, 0.000000000000000000 ) ) ;
#4762 = DIRECTION ( 'NONE',  ( 1.000000000000000000, 0.000000000000000000, 0.000000000000000000 ) ) ;
#4763 = DIRECTION ( 'NONE',  ( 0.000000000000000000, 1.000000000000000000, 0.000000000000000000 ) ) ;
#4764 = FACE_OUTER_BOUND ( 'NONE', #6449, .T. ) ;
#4765 = FACE_OUTER_BOUND ( 'NONE', #1021, .T. ) ;
#4766 = EDGE_CURVE ( 'NONE', #5732, #478, #2278, .T. ) ;
#4767 = ADVANCED_BREP_SHAPE_REPRESENTATION ( '', ( #5831, #1963 ), #4487 ) ;
#4768 = VERTEX_POINT ( 'NONE', #4083 ) ;
#4769 = CARTESIAN_POINT ( 'NONE',  ( 0.2500000000000002220, 5.204748896376250699E-16, -4.250000000000000000 ) ) ;
#4770 = ORIENTED_EDGE ( 'NONE', *, *, #4795, .F. ) ;
#4771 = SHAPE_REPRESENTATION ( 'base plate', ( #1963 ), #6040 ) ;
#4772 = CARTESIAN_POINT ( 'NONE',  ( -4.211405944401398038, -2.460460786169389902, -3.751298493805494072 ) ) ;
#4773 = ORIENTED_EDGE ( 'NONE', *, *, #6205, .F. ) ;
#4774 = ORIENTED_EDGE ( 'NONE', *, *, #6333, .F. ) ;
#4775 = APPLICATION_CONTEXT ( 'automotive_design' ) ;
#4776 = CYLINDRICAL_SURFACE ( 'NONE', #517, 2.649999999999985700 ) ;
#4777 = DIRECTION ( 'NONE',  ( -0.000000000000000000, -0.000000000000000000, 1.000000000000000000 ) ) ;
#4778 = EDGE_LOOP ( 'NONE', ( #5629, #3995, #6125, #1253, #7257 ) ) ;
#4779 = LINE ( 'NONE', #6511, #5822 ) ;
#4780 = ORIENTED_EDGE ( 'NONE', *, *, #4255, .T. ) ;
#4781 = ADVANCED_FACE ( 'NONE', ( #6973 ), #1934, .F. ) ;
#4782 = LINE ( 'NONE', #261, #2045 ) ;
#4783 = ITEM_DEFINED_TRANSFORMATION ( 'NONE', 'NONE', #4217,  #1963 ) ;
#4784 = CARTESIAN_POINT ( 'NONE',  ( 1.567478505476134606E-15, 4.618802153517012066, -3.433295621305382905 ) ) ;
#4785 = LINE ( 'NONE', #7010, #2681 ) ;
#4786 = ORIENTED_EDGE ( 'NONE', *, *, #958, .T. ) ;
#4787 = DIRECTION ( 'NONE',  ( -1.000000000000000000, 0.000000000000000000, 0.000000000000000000 ) ) ;
#4788 = EDGE_LOOP ( 'NONE', ( #5508, #1229, #7055, #357 ) ) ;
#4789 = PRODUCT_DEFINITION_SHAPE ( 'NONE', 'NONE',  #7398 ) ;
#4790 = ORIENTED_EDGE ( 'NONE', *, *, #623, .T. ) ;
#4791 = CARTESIAN_POINT ( 'NONE',  ( 155.0000000000000000, -8.660254037844389075, 139.9990000000000236 ) ) ;
#4792 = CARTESIAN_POINT ( 'NONE',  ( -0.5636800770129166693, -4.293361309317430319, -3.531542292955206275 ) ) ;
#4793 = CARTESIAN_POINT ( 'NONE',  ( 4.101954839143060028, 2.368264730582927857, -3.681130640444267854 ) ) ;
#4794 = CARTESIAN_POINT ( 'NONE',  ( 315.0000000000000568, 8.660254037844390851, 139.9990000000000236 ) ) ;
#4795 = EDGE_CURVE ( 'NONE', #2028, #2488, #2030, .T. ) ;
#4796 = CARTESIAN_POINT ( 'NONE',  ( 470.0000000000000000, -20.00000000000000000, 200.0000000000000000 ) ) ;
#4797 = CARTESIAN_POINT ( 'NONE',  ( 0.000000000000000000, 0.000000000000000000, -4.484454397937119197 ) ) ;
#4798 = EDGE_LOOP ( 'NONE', ( #3487, #6711, #4701, #5566 ) ) ;
#4799 = AXIS2_PLACEMENT_3D ( 'NONE', #5532, #6074, #6110 ) ;
#4800 = ITEM_DEFINED_TRANSFORMATION ( 'NONE', 'NONE', #552,  #1963 ) ;
#4801 = CARTESIAN_POINT ( 'NONE',  ( 0.000000000000000000, 0.000000000000000000, -140.0000000000000000 ) ) ;
#4802 = ORIENTED_EDGE ( 'NONE', *, *, #3390, .F. ) ;
#4803 = EDGE_CURVE ( 'NONE', #2803, #2072, #654, .T. ) ;
#4804 = VECTOR ( 'NONE', #2610, 999.9999999999998863 ) ;
#4805 = CARTESIAN_POINT ( 'NONE',  ( 155.0000000000000000, 8.660254037844390851, 139.9990000000000236 ) ) ;
#4806 = EDGE_LOOP ( 'NONE', ( #729, #5163, #6775, #3947 ) ) ;
#4807 = ORIENTED_EDGE ( 'NONE', *, *, #5953, .F. ) ;
#4808 = CARTESIAN_POINT ( 'NONE',  ( 4.999999999999999112, -8.660254037844389075, 145.0000000000000284 ) ) ;
#4809 = PRODUCT_DEFINITION_SHAPE ( 'NONE', 'NONE',  #7363 ) ;
#4810 = DIRECTION ( 'NONE',  ( -0.000000000000000000, -0.000000000000000000, -1.000000000000000000 ) ) ;
#4811 = VECTOR ( 'NONE', #5747, 1000.000000000000000 ) ;
#4812 = VECTOR ( 'NONE', #6999, 1000.000000000000000 ) ;
#4813 = CARTESIAN_POINT ( 'NONE',  ( 0.2500000000000002220, 0.000000000000000000, 0.000000000000000000 ) ) ;
#4814 = CARTESIAN_POINT ( 'NONE',  ( 315.0000000000000568, 8.660254037844390851, 140.0000000000000000 ) ) ;
#4815 = ORIENTED_EDGE ( 'NONE', *, *, #2889, .T. ) ;
#4816 = ADVANCED_FACE ( 'NONE', ( #5850 ), #128, .F. ) ;
#4817 = PRESENTATION_LAYER_ASSIGNMENT (  '', '', ( #6516 ) ) ;
#4818 = TOROIDAL_SURFACE ( 'NONE', #4945, 4.000000000000000000, 0.2500000000000000000 ) ;
#4819 = CARTESIAN_POINT ( 'NONE',  ( -20.63749999999999929, 0.000000000000000000, 0.000000000000000000 ) ) ;
#4820 = CARTESIAN_POINT ( 'NONE',  ( 303.3333333333333144, -15.00000000000000000, 165.1500000000000625 ) ) ;
#4821 = PLANE ( 'NONE',  #1490 ) ;
#4822 = ORIENTED_EDGE ( 'NONE', *, *, #3329, .T. ) ;
#4823 = AXIS2_PLACEMENT_3D ( 'NONE', #6842, #5082, #6282 ) ;
#4824 = DIRECTION ( 'NONE',  ( 0.000000000000000000, 0.000000000000000000, -1.000000000000000000 ) ) ;
#4825 = ORIENTED_EDGE ( 'NONE', *, *, #1774, .F. ) ;
#4826 = ORIENTED_EDGE ( 'NONE', *, *, #3890, .T. ) ;
#4827 =( REPRESENTATION_RELATIONSHIP ('NONE','NONE', #5587, #6025 ) REPRESENTATION_RELATIONSHIP_WITH_TRANSFORMATION ( #895 )SHAPE_REPRESENTATION_RELATIONSHIP( ) );
#4828 = LINE ( 'NONE', #7120, #1437 ) ;
#4829 = CARTESIAN_POINT ( 'NONE',  ( -1.800000000000001155, 1.628780242865979758E-15, 13.29999999999999893 ) ) ;
#4830 = AXIS2_PLACEMENT_3D ( 'NONE', #2415, #1860, #4718 ) ;
#4831 = CARTESIAN_POINT ( 'NONE',  ( 195.0000000000000000, 8.660254037844390851, 145.0000000000000284 ) ) ;
#4832 = CYLINDRICAL_SURFACE ( 'NONE', #64, 2.649999999999985700 ) ;
#4833 = FACE_OUTER_BOUND ( 'NONE', #245, .T. ) ;
#4834 = EDGE_CURVE ( 'NONE', #3461, #6988, #206, .T. ) ;
#4835 = CARTESIAN_POINT ( 'NONE',  ( 0.000000000000000000, 0.000000000000000000, 0.000000000000000000 ) ) ;
#4836 = VECTOR ( 'NONE', #4666, 1000.000000000000000 ) ;
#4837 = EDGE_CURVE ( 'NONE', #584, #3428, #3626, .T. ) ;
#4838 = ORIENTED_EDGE ( 'NONE', *, *, #3232, .F. ) ;
#4839 = PLANE ( 'NONE',  #3963 ) ;
#4840 = LINE ( 'NONE', #7165, #776 ) ;
#4841 = VERTEX_POINT ( 'NONE', #1895 ) ;
#4842 = CARTESIAN_POINT ( 'NONE',  ( 53.33333333333330017, -20.00000000000000000, 162.5000000000000853 ) ) ;
#4843 =( LENGTH_UNIT ( ) NAMED_UNIT ( * ) SI_UNIT ( .MILLI., .METRE. ) );
#4844 = AXIS2_PLACEMENT_3D ( 'NONE', #2251, #3251, #4548 ) ;
#4845 = PLANE ( 'NONE',  #3150 ) ;
#4846 = EDGE_CURVE ( 'NONE', #709, #4934, #5515, .T. ) ;
#4847 = EDGE_LOOP ( 'NONE', ( #199, #300, #292, #7091 ) ) ;
#4848 = ORIENTED_EDGE ( 'NONE', *, *, #1864, .T. ) ;
#4849 = CARTESIAN_POINT ( 'NONE',  ( 303.3333333333333144, -20.00000000000000000, 165.1500000000000625 ) ) ;
#4850 = CARTESIAN_POINT ( 'NONE',  ( 155.0000000000000000, 8.660254037844390851, 145.0000000000000284 ) ) ;
#4851 = CIRCLE ( 'NONE', #796, 2.649999999999985700 ) ;
#4852 = CYLINDRICAL_SURFACE ( 'NONE', #5299, 12.44999999999999929 ) ;
#4853 =( NAMED_UNIT ( * ) SI_UNIT ( $, .STERADIAN. ) SOLID_ANGLE_UNIT ( ) );
#4854 = EDGE_CURVE ( 'NONE', #5461, #3920, #4159, .T. ) ;
#4855 = ORIENTED_EDGE ( 'NONE', *, *, #430, .F. ) ;
#4856 = CARTESIAN_POINT ( 'NONE',  ( 386.6666666666666288, -20.00000000000000000, -165.1500000000000625 ) ) ;
#4857 = CONTEXT_DEPENDENT_SHAPE_REPRESENTATION ( #20, #4621 ) ;
#4858 = DIRECTION ( 'NONE',  ( 0.000000000000000000, 0.000000000000000000, -1.000000000000000000 ) ) ;
#4859 = FACE_OUTER_BOUND ( 'NONE', #5061, .T. ) ;
#4860 = DIRECTION ( 'NONE',  ( 6.123233995736766036E-17, -1.000000000000000000, 0.000000000000000000 ) ) ;
#4861 = PRESENTATION_LAYER_ASSIGNMENT (  '', '', ( #4522 ) ) ;
#4862 = VERTEX_POINT ( 'NONE', #6450 ) ;
#4863 = CARTESIAN_POINT ( 'NONE',  ( 4.000000000000000000, -2.309401076758514915, -3.433295621305383349 ) ) ;
#4864 = ORIENTED_EDGE ( 'NONE', *, *, #5739, .F. ) ;
#4865 = ORIENTED_EDGE ( 'NONE', *, *, #1026, .F. ) ;
#4866 = ORIENTED_EDGE ( 'NONE', *, *, #5219, .T. ) ;
#4867 = CARTESIAN_POINT ( 'NONE',  ( 2.500000000000000000, 2.357898499370433054, -1.951563910473907981E-15 ) ) ;
#4868 = DIRECTION ( 'NONE',  ( -1.000000000000000000, 0.000000000000000000, -0.000000000000000000 ) ) ;
#4869 = DIRECTION ( 'NONE',  ( -0.000000000000000000, -0.000000000000000000, 1.000000000000000000 ) ) ;
#4870 = CYLINDRICAL_SURFACE ( 'NONE', #546, 2.649999999999985700 ) ;
#4871 = DIRECTION ( 'NONE',  ( -0.000000000000000000, 1.000000000000000000, 0.000000000000000000 ) ) ;
#4872 = FACE_OUTER_BOUND ( 'NONE', #2810, .T. ) ;
#4873 =( REPRESENTATION_RELATIONSHIP ('NONE','NONE', #5587, #5294 ) REPRESENTATION_RELATIONSHIP_WITH_TRANSFORMATION ( #3557 )SHAPE_REPRESENTATION_RELATIONSHIP( ) );
#4874 = ORIENTED_EDGE ( 'NONE', *, *, #3511, .F. ) ;
#4875 = PRODUCT_DEFINITION_SHAPE ( 'NONE', 'NONE',  #7352 ) ;
#4876 = CARTESIAN_POINT ( 'NONE',  ( 5.384454397937118664, 0.000000000000000000, -5.000000000000000000 ) ) ;
#4877 = AXIS2_PLACEMENT_3D ( 'NONE', #1175, #3407, #583 ) ;
#4878 = LINE ( 'NONE', #3754, #651 ) ;
#4879 = ORIENTED_EDGE ( 'NONE', *, *, #3418, .T. ) ;
#4880 = EDGE_CURVE ( 'NONE', #3696, #6618, #4195, .T. ) ;
#4881 = CARTESIAN_POINT ( 'NONE',  ( 4.211140560182196957, 2.431303136016536470, -3.745885042887433514 ) ) ;
#4882 = CARTESIAN_POINT ( 'NONE',  ( 1.999999999999994893, 0.000000000000000000, -10.72499999999999964 ) ) ;
#4883 = LINE ( 'NONE', #4322, #7121 ) ;
#4884 = EDGE_LOOP ( 'NONE', ( #5928, #4039, #4606, #1102, #3545 ) ) ;
#4885 = DIRECTION ( 'NONE',  ( -1.000000000000000000, -6.123233995736766036E-17, -6.123233995736764803E-17 ) ) ;
#4886 = ORIENTED_EDGE ( 'NONE', *, *, #6042, .T. ) ;
#4887 = FACE_OUTER_BOUND ( 'NONE', #6947, .T. ) ;
#4888 = EDGE_CURVE ( 'NONE', #3129, #5338, #1242, .T. ) ;
#4889 = ADVANCED_FACE ( 'NONE', ( #2912 ), #2353, .F. ) ;
#4890 = CARTESIAN_POINT ( 'NONE',  ( 0.000000000000000000, 0.000000000000000000, -140.0000000000000000 ) ) ;
#4891 = CARTESIAN_POINT ( 'NONE',  ( 53.33333333333330017, -15.00000000000000000, 162.5000000000000853 ) ) ;
#4892 = ORIENTED_EDGE ( 'NONE', *, *, #1049, .F. ) ;
#4893 = DIRECTION ( 'NONE',  ( 0.000000000000000000, 0.4999999999999993339, -0.8660254037844390407 ) ) ;
#4894 = ITEM_DEFINED_TRANSFORMATION ( 'NONE', 'NONE', #5412,  #1963 ) ;
#4895 = LINE ( 'NONE', #4820, #5765 ) ;
#4896 = CARTESIAN_POINT ( 'NONE',  ( 124.9999999999999858, 8.660254037844390851, 139.9990000000000236 ) ) ;
#4897 = EDGE_CURVE ( 'NONE', #5434, #3802, #2648, .T. ) ;
#4898 = DIRECTION ( 'NONE',  ( -1.000000000000000000, 0.000000000000000000, 0.000000000000000000 ) ) ;
#4899 = ORIENTED_EDGE ( 'NONE', *, *, #6992, .F. ) ;
#4900 = FACE_BOUND ( 'NONE', #5385, .T. ) ;
#4901 = ADVANCED_FACE ( 'NONE', ( #2009 ), #3239, .F. ) ;
#4902 = AXIS2_PLACEMENT_3D ( 'NONE', #1133, #5657, #1063 ) ;
#4903 = ORIENTED_EDGE ( 'NONE', *, *, #5038, .F. ) ;
#4904 = B_SPLINE_CURVE_WITH_KNOTS ( 'NONE', 3,
 ( #1539, #3693, #5995, #6636, #6114, #3111, #2566, #2006 ),
 .UNSPECIFIED., .F., .F.,
 ( 4, 2, 2, 4 ),
 ( 0.000000000000000000, 0.002450665683189820997, 0.003675998524784731495, 0.004901331366379641993 ),
 .UNSPECIFIED. ) ;
#4905 = ORIENTED_EDGE ( 'NONE', *, *, #3499, .T. ) ;
#4906 = CARTESIAN_POINT ( 'NONE',  ( 13.50000000000000000, 0.000000000000000000, 121.0000000000000000 ) ) ;
#4907 = FACE_OUTER_BOUND ( 'NONE', #2693, .T. ) ;
#4908 = LINE ( 'NONE', #863, #742 ) ;
#4909 = DIRECTION ( 'NONE',  ( -0.000000000000000000, -0.000000000000000000, 1.000000000000000000 ) ) ;
#4910 = CIRCLE ( 'NONE', #844, 12.77499999999999858 ) ;
#4911 = CARTESIAN_POINT ( 'NONE',  ( -4.000000000000000000, -2.309401076758512694, -5.000000000000000000 ) ) ;
#4912 = DIRECTION ( 'NONE',  ( 0.000000000000000000, -0.000000000000000000, 1.000000000000000000 ) ) ;
#4913 = DIRECTION ( 'NONE',  ( 0.000000000000000000, 0.000000000000000000, -1.000000000000000000 ) ) ;
#4914 = ORIENTED_EDGE ( 'NONE', *, *, #4622, .F. ) ;
#4915 = VECTOR ( 'NONE', #5778, 1000.000000000000000 ) ;
#4916 = EDGE_CURVE ( 'NONE', #7081, #5855, #7276, .T. ) ;
#4917 = CARTESIAN_POINT ( 'NONE',  ( 0.000000000000000000, 0.000000000000000000, 140.0000000000000000 ) ) ;
#4918 = FACE_OUTER_BOUND ( 'NONE', #127, .T. ) ;
#4919 = ORIENTED_EDGE ( 'NONE', *, *, #3881, .T. ) ;
#4920 = DIRECTION ( 'NONE',  ( 1.000000000000000000, 0.000000000000000000, 0.000000000000000000 ) ) ;
#4921 = CARTESIAN_POINT ( 'NONE',  ( 2.290893957444128645E-15, 4.647089433458768681, -3.572167766733382877 ) ) ;
#4922 = CARTESIAN_POINT ( 'NONE',  ( 365.0000000000000000, -8.660254037844389075, 140.0000000000000000 ) ) ;
#4923 = ADVANCED_FACE ( 'NONE', ( #1424 ), #1977, .T. ) ;
#4924 = AXIS2_PLACEMENT_3D ( 'NONE', #6833, #5079, #4541 ) ;
#4925 = EDGE_LOOP ( 'NONE', ( #3151, #7058, #6805 ) ) ;
#4926 = DIRECTION ( 'NONE',  ( 1.000000000000000000, 0.000000000000000000, 0.000000000000000000 ) ) ;
#4927 = ORIENTED_EDGE ( 'NONE', *, *, #694, .T. ) ;
#4928 = CARTESIAN_POINT ( 'NONE',  ( 2.000000000000001776, 0.000000000000000000, 0.000000000000000000 ) ) ;
#4929 = VECTOR ( 'NONE', #2733, 1000.000000000000000 ) ;
#4930 = DIRECTION ( 'NONE',  ( 0.000000000000000000, 1.000000000000000000, 0.000000000000000000 ) ) ;
#4931 = CARTESIAN_POINT ( 'NONE',  ( 245.0000000000000000, -8.660254037844389075, 139.9990000000000236 ) ) ;
#4932 = EDGE_CURVE ( 'NONE', #6701, #2174, #792, .T. ) ;
#4933 = UNCERTAINTY_MEASURE_WITH_UNIT (LENGTH_MEASURE( 1.000000000000000082E-05 ), #4749, 'distance_accuracy_value', 'NONE');
#4934 = VERTEX_POINT ( 'NONE', #2694 ) ;
#4935 = EDGE_CURVE ( 'NONE', #6744, #1168, #1505, .T. ) ;
#4936 = CARTESIAN_POINT ( 'NONE',  ( 4.000000000000000000, -1.677850389431204459, -3.535268758346977513 ) ) ;
#4937 = VECTOR ( 'NONE', #6557, 1000.000000000000000 ) ;
#4938 = CARTESIAN_POINT ( 'NONE',  ( 2.500000000000000000, 2.357898499370433054, -1.951563910473907981E-15 ) ) ;
#4939 = DIRECTION ( 'NONE',  ( -0.000000000000000000, 0.000000000000000000, 1.000000000000000000 ) ) ;
#4940 = DIRECTION ( 'NONE',  ( 0.000000000000000000, 0.000000000000000000, 1.000000000000000000 ) ) ;
#4941 = ORIENTED_EDGE ( 'NONE', *, *, #1306, .T. ) ;
#4942 = CARTESIAN_POINT ( 'NONE',  ( 1.999999999999998224, -3.464101615137772594, -3.142992957459239012 ) ) ;
#4943 = PRODUCT_DEFINITION_SHAPE ( 'NONE', 'NONE',  #7359 ) ;
#4944 = CIRCLE ( 'NONE', #6984, 2.649999999999985700 ) ;
#4945 = AXIS2_PLACEMENT_3D ( 'NONE', #1464, #2103, #1428 ) ;
#4946 = EDGE_CURVE ( 'NONE', #3722, #1084, #4828, .T. ) ;
#4947 = CLOSED_SHELL ( 'NONE', ( #5264, #5250, #1326, #966, #2716, #2853, #5123, #3296, #2915, #5642, #6495, #301, #2261, #4058, #1993, #536, #608, #3105, #599, #6678, #4747, #6786, #487, #1751, #3946, #1272, #5479, #1610, #1852, #2770, #2035, #2255 ) ) ;
#4948 = ORIENTED_EDGE ( 'NONE', *, *, #3695, .F. ) ;
#4949 = ORIENTED_EDGE ( 'NONE', *, *, #7103, .F. ) ;
#4950 = CARTESIAN_POINT ( 'NONE',  ( 3.999999999999999112, -0.7890432684750902093, -0.04868663549882291247 ) ) ;
#4951 = CARTESIAN_POINT ( 'NONE',  ( 1.390230914382191596, 4.043987460488659202, -3.502507215260488582 ) ) ;
#4952 = DIRECTION ( 'NONE',  ( 0.000000000000000000, 0.000000000000000000, -1.000000000000000000 ) ) ;
#4953 = CARTESIAN_POINT ( 'NONE',  ( 405.0000000000000000, -8.660254037844389075, 139.9990000000000236 ) ) ;
#4954 = AXIS2_PLACEMENT_3D ( 'NONE', #927, #4409, #3144 ) ;
#4955 = AXIS2_PLACEMENT_3D ( 'NONE', #3090, #6602, #5393 ) ;
#4956 = AXIS2_PLACEMENT_3D ( 'NONE', #2872, #4047, #4020 ) ;
#4957 = DIRECTION ( 'NONE',  ( 0.000000000000000000, 0.000000000000000000, 1.000000000000000000 ) ) ;
#4958 = LINE ( 'NONE', #1981, #2410 ) ;
#4959 = ADVANCED_FACE ( 'NONE', ( #3663 ), #3737, .F. ) ;
#4960 = ORIENTED_EDGE ( 'NONE', *, *, #5609, .T. ) ;
#4961 = VECTOR ( 'NONE', #2847, 1000.000000000000000 ) ;
#4962 = COLOUR_RGB ( '',1.000000000000000000, 0.9490196078431372140, 0.9098039215686274384 ) ;
#4963 = CYLINDRICAL_SURFACE ( 'NONE', #256, 10.00000000000000000 ) ;
#4964 = CARTESIAN_POINT ( 'NONE',  ( 470.0000000000000000, -25.00000000000000000, 200.0000000000000000 ) ) ;
#4965 = CARTESIAN_POINT ( 'NONE',  ( 303.3333333333333144, -20.00000000000000000, 162.5000000000000853 ) ) ;
#4966 = SURFACE_SIDE_STYLE ('',( #2905 ) ) ;
#4967 = AXIS2_PLACEMENT_3D ( 'NONE', #2277, #4575, #6313 ) ;
#4968 = DIRECTION ( 'NONE',  ( 1.000000000000000000, 0.000000000000000000, 0.000000000000000000 ) ) ;
#4969 = AXIS2_PLACEMENT_3D ( 'NONE', #1548, #6088, #3824 ) ;
#4970 = CARTESIAN_POINT ( 'NONE',  ( 235.0000000000000000, -8.660254037844389075, 139.9990000000000236 ) ) ;
#4971 = VERTEX_POINT ( 'NONE', #6082 ) ;
#4972 = ORIENTED_EDGE ( 'NONE', *, *, #660, .F. ) ;
#4973 = ADVANCED_FACE ( 'NONE', ( #3782 ), #5863, .F. ) ;
#4974 = DIRECTION ( 'NONE',  ( 6.123233995736766036E-17, -1.000000000000000000, 0.000000000000000000 ) ) ;
#4975 = VECTOR ( 'NONE', #2076, 1000.000000000000000 ) ;
#4976 = EDGE_LOOP ( 'NONE', ( #6363, #3528, #981 ) ) ;
#4977 = AXIS2_PLACEMENT_3D ( 'NONE', #3950, #480, #2814 ) ;
#4978 = DIRECTION ( 'NONE',  ( 1.000000000000000000, 0.000000000000000000, 0.000000000000000000 ) ) ;
#4979 = CARTESIAN_POINT ( 'NONE',  ( 285.0000000000000568, -8.660254037844389075, 145.0000000000000284 ) ) ;
#4980 = CARTESIAN_POINT ( 'NONE',  ( 0.2277608394786177770, 0.000000000000000000, 0.000000000000000000 ) ) ;
#4981 = VECTOR ( 'NONE', #3976, 1000.000000000000000 ) ;
#4982 = EDGE_LOOP ( 'NONE', ( #3765, #1052, #3442, #2449 ) ) ;
#4983 = FACE_BOUND ( 'NONE', #488, .T. ) ;
#4984 = ADVANCED_FACE ( 'NONE', ( #4270 ), #6468, .T. ) ;
#4985 = ITEM_DEFINED_TRANSFORMATION ( 'NONE', 'NONE', #7222,  #1963 ) ;
#4986 = PLANE ( 'NONE',  #3847 ) ;
#4987 = DIRECTION ( 'NONE',  ( 1.000000000000000000, 0.000000000000000000, 0.000000000000000000 ) ) ;
#4988 = CIRCLE ( 'NONE', #569, 10.00000000000000000 ) ;
#4989 = DIRECTION ( 'NONE',  ( 0.000000000000000000, 0.000000000000000000, 1.000000000000000000 ) ) ;
#4990 =( REPRESENTATION_RELATIONSHIP ('NONE','NONE', #5587, #5294 ) REPRESENTATION_RELATIONSHIP_WITH_TRANSFORMATION ( #3849 )SHAPE_REPRESENTATION_RELATIONSHIP( ) );
#4991 = ORIENTED_EDGE ( 'NONE', *, *, #1115, .F. ) ;
#4992 = DIRECTION ( 'NONE',  ( -0.000000000000000000, 0.000000000000000000, 1.000000000000000000 ) ) ;
#4993 = VERTEX_POINT ( 'NONE', #6044 ) ;
#4994 = VERTEX_POINT ( 'NONE', #7235 ) ;
#4995 = DIRECTION ( 'NONE',  ( 1.000000000000000000, 0.000000000000000000, -0.000000000000000000 ) ) ;
#4996 = CARTESIAN_POINT ( 'NONE',  ( 136.6666666666666288, -25.00000000000000000, -162.5000000000000853 ) ) ;
#4997 = CONTEXT_DEPENDENT_SHAPE_REPRESENTATION ( #7284, #4809 ) ;
#4998 = CARTESIAN_POINT ( 'NONE',  ( -4.000000000000000000, 0.000000000000000000, 0.000000000000000000 ) ) ;
#4999 = LINE ( 'NONE', #6719, #6761 ) ;
#5000 = EDGE_CURVE ( 'NONE', #468, #6247, #1313, .T. ) ;
#5001 = DIRECTION ( 'NONE',  ( 0.000000000000000000, -0.5000000000000011102, -0.8660254037844379305 ) ) ;
#5002 = LINE ( 'NONE', #6004, #6503 ) ;
#5003 = VERTEX_POINT ( 'NONE', #6716 ) ;
#5004 = CARTESIAN_POINT ( 'NONE',  ( 470.0000000000000000, -25.00000000000000000, 200.0000000000000000 ) ) ;
#5005 = CARTESIAN_POINT ( 'NONE',  ( -30.00000000000000000, 0.000000000000000000, 140.0000000000000000 ) ) ;
#5006 = PLANE ( 'NONE',  #3214 ) ;
#5007 = DIRECTION ( 'NONE',  ( 0.000000000000000000, 1.000000000000000000, -1.224646799147353207E-16 ) ) ;
#5008 =( NAMED_UNIT ( * ) SI_UNIT ( $, .STERADIAN. ) SOLID_ANGLE_UNIT ( ) );
#5009 = EDGE_CURVE ( 'NONE', #6725, #1598, #7194, .T. ) ;
#5010 = SURFACE_STYLE_USAGE ( .BOTH. , #2709 ) ;
#5011 = EDGE_LOOP ( 'NONE', ( #2672, #7246, #3542, #6859 ) ) ;
#5012 = DIRECTION ( 'NONE',  ( -1.000000000000000000, -0.000000000000000000, -0.000000000000000000 ) ) ;
#5013 = EDGE_LOOP ( 'NONE', ( #1340, #5137 ) ) ;
#5014 = CARTESIAN_POINT ( 'NONE',  ( 400.0000000000000000, 0.000000000000000000, 123.0000000000000000 ) ) ;
#5015 = ORIENTED_EDGE ( 'NONE', *, *, #2735, .F. ) ;
#5016 = DIRECTION ( 'NONE',  ( 1.000000000000000000, 0.000000000000000000, 0.000000000000000000 ) ) ;
#5017 = DIRECTION ( 'NONE',  ( -1.000000000000000000, 0.000000000000000000, -0.000000000000000000 ) ) ;
#5018 = LINE ( 'NONE', #457, #5704 ) ;
#5019 = VERTEX_POINT ( 'NONE', #905 ) ;
#5020 = CARTESIAN_POINT ( 'NONE',  ( -5.000000000000000888, -8.660254037844389075, 139.9990000000000236 ) ) ;
#5021 = CARTESIAN_POINT ( 'NONE',  ( 0.3198814748697593746, 4.434118497892183264, -0.3507732604232499107 ) ) ;
#5022 = LINE ( 'NONE', #5101, #1258 ) ;
#5023 = SHAPE_REPRESENTATION ( 'hex flange nut gradea_iso_ISO - 4161 - M5 - N', ( #1963 ), #4487 ) ;
#5024 = CARTESIAN_POINT ( 'NONE',  ( 0.000000000000000000, 0.000000000000000000, 0.000000000000000000 ) ) ;
#5025 = ORIENTED_EDGE ( 'NONE', *, *, #4946, .F. ) ;
#5026 = EDGE_CURVE ( 'NONE', #3704, #5368, #3162, .T. ) ;
#5027 = ORIENTED_EDGE ( 'NONE', *, *, #5520, .T. ) ;
#5028 = ORIENTED_EDGE ( 'NONE', *, *, #2154, .F. ) ;
#5029 = FACE_OUTER_BOUND ( 'NONE', #3342, .T. ) ;
#5030 = CARTESIAN_POINT ( 'NONE',  ( 355.0000000000000000, -8.660254037844389075, 140.0000000000000000 ) ) ;
#5031 = CONTEXT_DEPENDENT_SHAPE_REPRESENTATION ( #3137, #2591 ) ;
#5032 = LINE ( 'NONE', #435, #2644 ) ;
#5033 = LINE ( 'NONE', #6908, #5921 ) ;
#5034 = DIRECTION ( 'NONE',  ( 0.000000000000000000, 0.000000000000000000, -1.000000000000000000 ) ) ;
#5035 = PRODUCT_DEFINITION_CONTEXT ( 'detailed design', #3620, 'design' ) ;
#5036 = CARTESIAN_POINT ( 'NONE',  ( 235.0000000000000000, 8.660254037844390851, 145.0000000000000284 ) ) ;
#5037 = ORIENTED_EDGE ( 'NONE', *, *, #1222, .F. ) ;
#5038 = EDGE_CURVE ( 'NONE', #6651, #2247, #5500, .T. ) ;
#5039 = CYLINDRICAL_SURFACE ( 'NONE', #3967, 2.649999999999985700 ) ;
#5040 = FACE_OUTER_BOUND ( 'NONE', #6913, .T. ) ;
#5041 = CARTESIAN_POINT ( 'NONE',  ( -1.654252653721913102, -3.663718938583024443, -0.01223254789874440342 ) ) ;
#5042 =( NAMED_UNIT ( * ) SI_UNIT ( $, .STERADIAN. ) SOLID_ANGLE_UNIT ( ) );
#5043 = LINE ( 'NONE', #2067, #4333 ) ;
#5044 = ADVANCED_BREP_SHAPE_REPRESENTATION ( '', ( #856, #1963 ), #5797 ) ;
#5045 = B_SPLINE_CURVE_WITH_KNOTS ( 'NONE', 3,
 ( #693, #1795, #4086, #754, #168, #1836 ),
 .UNSPECIFIED., .F., .F.,
 ( 4, 2, 4 ),
 ( 0.002365888236227977302, 0.003551327329835078910, 0.004736766423442180518 ),
 .UNSPECIFIED. ) ;
#5046 = ORIENTED_EDGE ( 'NONE', *, *, #4059, .F. ) ;
#5047 = ORIENTED_EDGE ( 'NONE', *, *, #3283, .F. ) ;
#5048 = EDGE_CURVE ( 'NONE', #5003, #2185, #2049, .T. ) ;
#5049 = CARTESIAN_POINT ( 'NONE',  ( 303.3333333333333144, -10.00000000000000178, -162.5000000000000853 ) ) ;
#5050 = ORIENTED_EDGE ( 'NONE', *, *, #6689, .F. ) ;
#5051 = CARTESIAN_POINT ( 'NONE',  ( 445.0000000000000000, 8.660254037844390851, 139.9990000000000236 ) ) ;
#5052 = ADVANCED_FACE ( 'NONE', ( #982 ), #3570, .T. ) ;
#5053 = DIRECTION ( 'NONE',  ( 1.000000000000000000, 0.000000000000000000, 0.000000000000000000 ) ) ;
#5054 = ORIENTED_EDGE ( 'NONE', *, *, #3458, .F. ) ;
#5055 = CARTESIAN_POINT ( 'NONE',  ( 45.00000000000000000, -8.660254037844389075, 140.0000000000000000 ) ) ;
#5056 = AXIS2_PLACEMENT_3D ( 'NONE', #3099, #5405, #1629 ) ;
#5057 = CARTESIAN_POINT ( 'NONE',  ( 2.500000000000000000, -2.629050547790028551E-15, -2.041999999999999815 ) ) ;
#5058 = CIRCLE ( 'NONE', #2173, 4.250000000000000000 ) ;
#5059 = CARTESIAN_POINT ( 'NONE',  ( 2.500000000000000000, 1.178949249685213863, -2.042000000000001148 ) ) ;
#5060 = DIRECTION ( 'NONE',  ( 1.000000000000000000, 0.000000000000000000, 0.000000000000000000 ) ) ;
#5061 = EDGE_LOOP ( 'NONE', ( #1110, #4357, #5926, #1152 ) ) ;
#5062 = DIRECTION ( 'NONE',  ( -1.000000000000000000, 0.000000000000000000, 0.000000000000000000 ) ) ;
#5063 = EDGE_CURVE ( 'NONE', #4768, #6751, #5603, .T. ) ;
#5064 = ORIENTED_EDGE ( 'NONE', *, *, #5776, .T. ) ;
#5065 = CIRCLE ( 'NONE', #640, 10.00000000000000000 ) ;
#5066 = EDGE_LOOP ( 'NONE', ( #102, #2607, #2183, #7296 ) ) ;
#5067 = CARTESIAN_POINT ( 'NONE',  ( 386.6666666666666288, -20.00000000000000000, 162.5000000000000853 ) ) ;
#5068 = CARTESIAN_POINT ( 'NONE',  ( -4.203833317240879275, -1.627343821129593859, -3.597273115243890818 ) ) ;
#5069 = CARTESIAN_POINT ( 'NONE',  ( -1.799999999999996048, 1.224646799147353059E-15, 9.999999999999998224 ) ) ;
#5070 = CARTESIAN_POINT ( 'NONE',  ( 219.9999999999999716, -14.99999999999999822, 159.8500000000001080 ) ) ;
#5071 = VECTOR ( 'NONE', #1868, 1000.000000000000000 ) ;
#5072 = DIRECTION ( 'NONE',  ( 0.8660254037844374864, -0.5000000000000018874, 0.000000000000000000 ) ) ;
#5073 = AXIS2_PLACEMENT_3D ( 'NONE', #2830, #5615, #2267 ) ;
#5074 = CLOSED_SHELL ( 'NONE', ( #3649, #4654, #5666, #331, #832, #6368, #2487, #205, #6403, #4545, #2541, #740, #1352, #627, #94, #613, #5494, #4816, #3834, #1743 ) ) ;
#5075 = ORIENTED_EDGE ( 'NONE', *, *, #2791, .T. ) ;
#5076 = AXIS2_PLACEMENT_3D ( 'NONE', #2412, #1785, #4073 ) ;
#5077 = FACE_OUTER_BOUND ( 'NONE', #5569, .T. ) ;
#5078 = LINE ( 'NONE', #5005, #7247 ) ;
#5079 = DIRECTION ( 'NONE',  ( -0.000000000000000000, -0.000000000000000000, -1.000000000000000000 ) ) ;
#5080 = AXIS2_PLACEMENT_3D ( 'NONE', #1547, #6203, #1463 ) ;
#5081 = CARTESIAN_POINT ( 'NONE',  ( 136.6666666666666288, -20.00000000000000000, 162.5000000000000853 ) ) ;
#5082 = DIRECTION ( 'NONE',  ( -0.000000000000000000, 1.000000000000000000, -0.000000000000000000 ) ) ;
#5083 = AXIS2_PLACEMENT_3D ( 'NONE', #2172, #1140, #1622 ) ;
#5084 = AXIS2_PLACEMENT_3D ( 'NONE', #5409, #5017, #371 ) ;
#5085 = EDGE_CURVE ( 'NONE', #6352, #6894, #2206, .T. ) ;
#5086 = CARTESIAN_POINT ( 'NONE',  ( 164.9999999999999716, 8.660254037844390851, 139.9990000000000236 ) ) ;
#5087 = AXIS2_PLACEMENT_3D ( 'NONE', #6901, #1199, #6307 ) ;
#5088 = ORIENTED_EDGE ( 'NONE', *, *, #6657, .T. ) ;
#5089 = VERTEX_POINT ( 'NONE', #1616 ) ;
#5090 = ORIENTED_EDGE ( 'NONE', *, *, #1730, .F. ) ;
#5091 =( REPRESENTATION_RELATIONSHIP ('NONE','NONE', #5587, #1193 ) REPRESENTATION_RELATIONSHIP_WITH_TRANSFORMATION ( #6799 )SHAPE_REPRESENTATION_RELATIONSHIP( ) );
#5092 = CIRCLE ( 'NONE', #2904, 2.100000000000000089 ) ;
#5093 = AXIS2_PLACEMENT_3D ( 'NONE', #1680, #6257, #574 ) ;
#5094 = EDGE_CURVE ( 'NONE', #5816, #76, #1482, .T. ) ;
#5095 = FACE_OUTER_BOUND ( 'NONE', #6446, .T. ) ;
#5096 = VECTOR ( 'NONE', #4495, 1000.000000000000227 ) ;
#5097 = EDGE_LOOP ( 'NONE', ( #1451, #4146, #6849, #1185 ) ) ;
#5098 = CIRCLE ( 'NONE', #77, 1.050000000000000488 ) ;
#5099 = DIRECTION ( 'NONE',  ( 1.000000000000000000, 0.000000000000000000, 0.000000000000000000 ) ) ;
#5100 = FACE_BOUND ( 'NONE', #2538, .T. ) ;
#5101 = CARTESIAN_POINT ( 'NONE',  ( 470.0000000000000000, -20.00000000000000000, 200.0000000000000000 ) ) ;
#5102 = DIRECTION ( 'NONE',  ( 0.000000000000000000, 0.000000000000000000, 1.000000000000000000 ) ) ;
#5103 = EDGE_CURVE ( 'NONE', #563, #2630, #3859, .T. ) ;
#5104 = AXIS2_PLACEMENT_3D ( 'NONE', #862, #5428, #4307 ) ;
#5105 = EDGE_LOOP ( 'NONE', ( #293, #3813, #5944, #1405 ) ) ;
#5106 = DIRECTION ( 'NONE',  ( 0.000000000000000000, 0.000000000000000000, 1.000000000000000000 ) ) ;
#5107 = ORIENTED_EDGE ( 'NONE', *, *, #4576, .T. ) ;
#5108 = DIRECTION ( 'NONE',  ( -0.000000000000000000, 1.000000000000000000, -0.000000000000000000 ) ) ;
#5109 = AXIS2_PLACEMENT_3D ( 'NONE', #1655, #6641, #6682 ) ;
#5110 = CARTESIAN_POINT ( 'NONE',  ( 2.000000000000001776, 0.000000000000000000, 0.000000000000000000 ) ) ;
#5111 = CARTESIAN_POINT ( 'NONE',  ( 303.3333333333333144, -20.00000000000000000, 159.8500000000001080 ) ) ;
#5112 = CARTESIAN_POINT ( 'NONE',  ( 435.0000000000000568, 8.660254037844390851, 140.0000000000000000 ) ) ;
#5113 = PRODUCT_RELATED_PRODUCT_CATEGORY ( 'part', '', ( #3604 ) ) ;
#5114 = ORIENTED_EDGE ( 'NONE', *, *, #419, .T. ) ;
#5115 = ORIENTED_EDGE ( 'NONE', *, *, #1693, .T. ) ;
#5116 = CARTESIAN_POINT ( 'NONE',  ( 0.000000000000000000, -20.00000000000000000, 0.000000000000000000 ) ) ;
#5117 = DIRECTION ( 'NONE',  ( 0.000000000000000000, 0.000000000000000000, 1.000000000000000000 ) ) ;
#5118 = FACE_OUTER_BOUND ( 'NONE', #3714, .T. ) ;
#5119 = FACE_BOUND ( 'NONE', #604, .T. ) ;
#5120 = CARTESIAN_POINT ( 'NONE',  ( 4.999999999999999112, 8.660254037844390851, 150.0000000000000000 ) ) ;
#5121 = ORIENTED_EDGE ( 'NONE', *, *, #3843, .F. ) ;
#5122 = ORIENTED_EDGE ( 'NONE', *, *, #3248, .T. ) ;
#5123 = ADVANCED_FACE ( 'NONE', ( #2243 ), #6830, .F. ) ;
#5124 = CARTESIAN_POINT ( 'NONE',  ( 400.0000000000000000, 0.000000000000000000, -123.0000000000000000 ) ) ;
#5125 = EDGE_LOOP ( 'NONE', ( #1457, #1307, #3971, #5692 ) ) ;
#5126 = CARTESIAN_POINT ( 'NONE',  ( 114.9999999999999858, 8.660254037844390851, 140.0000000000000000 ) ) ;
#5127 = CARTESIAN_POINT ( 'NONE',  ( 45.00000000000000000, 8.660254037844390851, 139.9990000000000236 ) ) ;
#5128 = VERTEX_POINT ( 'NONE', #6263 ) ;
#5129 = APPLICATION_CONTEXT ( 'automotive_design' ) ;
#5130 = ADVANCED_FACE ( 'NONE', ( #3286 ), #6158, .F. ) ;
#5131 = FACE_BOUND ( 'NONE', #1515, .T. ) ;
#5132 = CARTESIAN_POINT ( 'NONE',  ( 0.000000000000000000, 0.000000000000000000, 0.000000000000000000 ) ) ;
#5133 = EDGE_CURVE ( 'NONE', #2792, #6365, #503, .T. ) ;
#5134 = CARTESIAN_POINT ( 'NONE',  ( 40.00000000000000000, 0.000000000000000000, 0.000000000000000000 ) ) ;
#5135 = ORIENTED_EDGE ( 'NONE', *, *, #4209, .T. ) ;
#5136 = CARTESIAN_POINT ( 'NONE',  ( 4.999999999999999112, 8.660254037844390851, 150.0000000000000000 ) ) ;
#5137 = ORIENTED_EDGE ( 'NONE', *, *, #430, .T. ) ;
#5138 = EDGE_CURVE ( 'NONE', #1780, #2884, #4555, .T. ) ;
#5139 = CARTESIAN_POINT ( 'NONE',  ( 0.2500000000000002220, 0.000000000000000000, 0.000000000000000000 ) ) ;
#5140 = DIRECTION ( 'NONE',  ( 0.000000000000000000, 0.000000000000000000, 1.000000000000000000 ) ) ;
#5141 = ITEM_DEFINED_TRANSFORMATION ( 'NONE', 'NONE', #411,  #1963 ) ;
#5142 = LINE ( 'NONE', #1688, #987 ) ;
#5143 = DIRECTION ( 'NONE',  ( 1.000000000000000000, 0.000000000000000000, 0.000000000000000000 ) ) ;
#5144 = VERTEX_POINT ( 'NONE', #3403 ) ;
#5145 = CARTESIAN_POINT ( 'NONE',  ( 303.3333333333333144, -20.00000000000000000, 162.5000000000000853 ) ) ;
#5146 = ORIENTED_EDGE ( 'NONE', *, *, #1875, .F. ) ;
#5147 = CARTESIAN_POINT ( 'NONE',  ( -5.000000000000000888, 8.660254037844390851, 139.9990000000000236 ) ) ;
#5148 = CARTESIAN_POINT ( 'NONE',  ( 0.02448733951239481094, 4.877042772274728044, -3.751161874094022242 ) ) ;
#5149 = DIRECTION ( 'NONE',  ( -0.000000000000000000, -0.000000000000000000, 1.000000000000000000 ) ) ;
#5150 =( NAMED_UNIT ( * ) SI_UNIT ( $, .STERADIAN. ) SOLID_ANGLE_UNIT ( ) );
#5151 = ADVANCED_FACE ( 'NONE', ( #3360, #5029 ), #1027, .T. ) ;
#5152 = ORIENTED_EDGE ( 'NONE', *, *, #2368, .T. ) ;
#5153 = DIRECTION ( 'NONE',  ( -1.000000000000000000, 0.000000000000000000, 0.000000000000000000 ) ) ;
#5154 = ORIENTED_EDGE ( 'NONE', *, *, #184, .T. ) ;
#5155 = PRODUCT_DEFINITION_SHAPE ( 'NONE', 'NONE',  #7385 ) ;
#5156 = VECTOR ( 'NONE', #3870, 1000.000000000000000 ) ;
#5157 = CARTESIAN_POINT ( 'NONE',  ( 1.999999999999998224, 0.000000000000000000, 0.000000000000000000 ) ) ;
#5158 = ORIENTED_EDGE ( 'NONE', *, *, #5865, .F. ) ;
#5159 = CARTESIAN_POINT ( 'NONE',  ( 2.000000000000001332, 13.29999999999999893, 0.000000000000000000 ) ) ;
#5160 = LINE ( 'NONE', #5059, #3514 ) ;
#5161 = CARTESIAN_POINT ( 'NONE',  ( 136.6666666666666288, -30.00000000000000355, -162.5000000000000853 ) ) ;
#5162 = EDGE_CURVE ( 'NONE', #6179, #4054, #1900, .T. ) ;
#5163 = ORIENTED_EDGE ( 'NONE', *, *, #635, .T. ) ;
#5164 = CARTESIAN_POINT ( 'NONE',  ( -4.204015924366189871, 1.626724848190922446, -3.610627190413390419 ) ) ;
#5165 = EDGE_CURVE ( 'NONE', #6755, #6469, #542, .T. ) ;
#5166 = CIRCLE ( 'NONE', #4688, 2.649999999999985700 ) ;
#5167 = EDGE_LOOP ( 'NONE', ( #5522, #6792, #3160, #4927 ) ) ;
#5168 = DIRECTION ( 'NONE',  ( 1.000000000000000000, 0.000000000000000000, 0.000000000000000000 ) ) ;
#5169 = PLANE ( 'NONE',  #4377 ) ;
#5170 = ITEM_DEFINED_TRANSFORMATION ( 'NONE', 'NONE', #5687,  #1963 ) ;
#5171 = DIRECTION ( 'NONE',  ( 0.000000000000000000, 1.000000000000000000, 0.000000000000000000 ) ) ;
#5172 = CARTESIAN_POINT ( 'NONE',  ( 155.0000000000000000, -8.660254037844389075, 145.0000000000000284 ) ) ;
#5173 = VECTOR ( 'NONE', #3118, 1000.000000000000000 ) ;
#5174 = ORIENTED_EDGE ( 'NONE', *, *, #6465, .F. ) ;
#5175 = CARTESIAN_POINT ( 'NONE',  ( 4.198928548860774157, -0.8158838809860124996, -3.526471437616918170 ) ) ;
#5176 = EDGE_CURVE ( 'NONE', #4054, #6179, #4301, .T. ) ;
#5177 = ORIENTED_EDGE ( 'NONE', *, *, #5695, .T. ) ;
#5178 = DIRECTION ( 'NONE',  ( -1.000000000000000000, -0.000000000000000000, -0.000000000000000000 ) ) ;
#5179 = FACE_OUTER_BOUND ( 'NONE', #5849, .T. ) ;
#5180 = CARTESIAN_POINT ( 'NONE',  ( 45.00000000000000000, 8.660254037844390851, 145.0000000000000284 ) ) ;
#5181 = LINE ( 'NONE', #3552, #6635 ) ;
#5182 = CIRCLE ( 'NONE', #1117, 4.000000000000000000 ) ;
#5183 = CARTESIAN_POINT ( 'NONE',  ( -2.100000000000000089, 2.571758278209441957E-16, -4.694516984716113228 ) ) ;
#5184 = EDGE_CURVE ( 'NONE', #2174, #2565, #7063, .T. ) ;
#5185 = PRODUCT_DEFINITION_FORMATION_WITH_SPECIFIED_SOURCE ( 'ANY', '', #3544, .NOT_KNOWN. ) ;
#5186 = ORIENTED_EDGE ( 'NONE', *, *, #4694, .T. ) ;
#5187 = CIRCLE ( 'NONE', #758, 2.649999999999985700 ) ;
#5188 = APPLICATION_PROTOCOL_DEFINITION ( 'draft international standard', 'automotive_design', 1998, #5493 ) ;
#5189 = ORIENTED_EDGE ( 'NONE', *, *, #1510, .T. ) ;
#5190 = CIRCLE ( 'NONE', #3391, 13.50000000000000178 ) ;
#5191 = AXIS2_PLACEMENT_3D ( 'NONE', #6860, #1479, #2240 ) ;
#5192 = PLANE ( 'NONE',  #1975 ) ;
#5193 = ORIENTED_EDGE ( 'NONE', *, *, #3536, .F. ) ;
#5194 = AXIS2_PLACEMENT_3D ( 'NONE', #3440, #2808, #5738 ) ;
#5195 = COLOUR_RGB ( '',0.8941176470588234615, 0.8941176470588234615, 0.8941176470588234615 ) ;
#5196 = LINE ( 'NONE', #4143, #3764 ) ;
#5197 = VERTEX_POINT ( 'NONE', #5735 ) ;
#5198 = VECTOR ( 'NONE', #3147, 1000.000000000000000 ) ;
#5199 = PRESENTATION_STYLE_ASSIGNMENT (( #6438 ) ) ;
#5200 = ORIENTED_EDGE ( 'NONE', *, *, #6321, .T. ) ;
#5201 = EDGE_CURVE ( 'NONE', #2247, #7016, #5260, .T. ) ;
#5202 = ORIENTED_EDGE ( 'NONE', *, *, #3273, .F. ) ;
#5203 = DIRECTION ( 'NONE',  ( 0.000000000000000000, 0.000000000000000000, 1.000000000000000000 ) ) ;
#5204 = DIRECTION ( 'NONE',  ( 1.000000000000000000, 0.000000000000000000, 0.000000000000000000 ) ) ;
#5205 =( GEOMETRIC_REPRESENTATION_CONTEXT ( 3 ) GLOBAL_UNCERTAINTY_ASSIGNED_CONTEXT ( ( #5336 ) ) GLOBAL_UNIT_ASSIGNED_CONTEXT ( ( #6325, #5295, #1747 ) ) REPRESENTATION_CONTEXT ( 'NONE', 'WORKASPACE' ) );
#5206 = LINE ( 'NONE', #505, #2637 ) ;
#5207 = DIRECTION ( 'NONE',  ( 0.000000000000000000, 0.000000000000000000, -1.000000000000000000 ) ) ;
#5208 = VECTOR ( 'NONE', #959, 1000.000000000000000 ) ;
#5209 = APPLICATION_PROTOCOL_DEFINITION ( 'draft international standard', 'automotive_design', 1998, #678 ) ;
#5210 = ORIENTED_EDGE ( 'NONE', *, *, #4449, .F. ) ;
#5211 = CARTESIAN_POINT ( 'NONE',  ( -2.449848172108560540, -3.432307619358754724, -3.503702292528910078 ) ) ;
#5212 = ORIENTED_EDGE ( 'NONE', *, *, #6465, .T. ) ;
#5213 = CIRCLE ( 'NONE', #3903, 13.50000000000000533 ) ;
#5214 = PRODUCT_DEFINITION_SHAPE ( 'NONE', 'NONE',  #7406 ) ;
#5215 = PLANE ( 'NONE',  #733 ) ;
#5216 = LINE ( 'NONE', #99, #2688 ) ;
#5217 = DIRECTION ( 'NONE',  ( 1.000000000000000000, 0.000000000000000000, -0.000000000000000000 ) ) ;
#5218 = LINE ( 'NONE', #66, #1012 ) ;
#5219 = EDGE_CURVE ( 'NONE', #2884, #1004, #609, .T. ) ;
#5220 = VECTOR ( 'NONE', #3268, 1000.000000000000000 ) ;
#5221 = LINE ( 'NONE', #2254, #2408 ) ;
#5222 =( REPRESENTATION_RELATIONSHIP ('NONE','NONE', #5587, #1193 ) REPRESENTATION_RELATIONSHIP_WITH_TRANSFORMATION ( #4783 )SHAPE_REPRESENTATION_RELATIONSHIP( ) );
#5223 = ORIENTED_EDGE ( 'NONE', *, *, #2179, .F. ) ;
#5224 = ORIENTED_EDGE ( 'NONE', *, *, #4694, .F. ) ;
#5225 = PRODUCT_CONTEXT ( 'NONE', #5493, 'mechanical' ) ;
#5226 = DIRECTION ( 'NONE',  ( 0.000000000000000000, 1.000000000000000000, 0.000000000000000000 ) ) ;
#5227 = VERTEX_POINT ( 'NONE', #2865 ) ;
#5228 = EDGE_CURVE ( 'NONE', #6651, #1304, #3694, .T. ) ;
#5229 = CARTESIAN_POINT ( 'NONE',  ( 0.000000000000000000, 0.000000000000000000, 200.0000000000000000 ) ) ;
#5230 = ORIENTED_EDGE ( 'NONE', *, *, #5176, .T. ) ;
#5231 = CARTESIAN_POINT ( 'NONE',  ( -2.687328764639638656, 3.067272167851286202, -0.05923475698270370959 ) ) ;
#5232 = CARTESIAN_POINT ( 'NONE',  ( -13.50000000000000000, 1.653273178848926867E-15, 125.0000000000000000 ) ) ;
#5233 = LINE ( 'NONE', #116, #2411 ) ;
#5234 = DIRECTION ( 'NONE',  ( 0.000000000000000000, -0.000000000000000000, 1.000000000000000000 ) ) ;
#5235 = ORIENTED_EDGE ( 'NONE', *, *, #2783, .F. ) ;
#5236 = CARTESIAN_POINT ( 'NONE',  ( -4.197393957002303999, -0.8151795401431414234, -3.503767560748935139 ) ) ;
#5237 = LINE ( 'NONE', #5840, #2490 ) ;
#5238 = FACE_BOUND ( 'NONE', #1155, .T. ) ;
#5239 = FACE_OUTER_BOUND ( 'NONE', #2118, .T. ) ;
#5240 = DIRECTION ( 'NONE',  ( 0.000000000000000000, 0.000000000000000000, 1.000000000000000000 ) ) ;
#5241 = ORIENTED_EDGE ( 'NONE', *, *, #2815, .T. ) ;
#5242 = CARTESIAN_POINT ( 'NONE',  ( 0.000000000000000000, 0.000000000000000000, -4.000000000000000000 ) ) ;
#5243 = ADVANCED_FACE ( 'NONE', ( #3002 ), #2747, .T. ) ;
#5244 = ORIENTED_EDGE ( 'NONE', *, *, #4766, .F. ) ;
#5245 = DIRECTION ( 'NONE',  ( 0.000000000000000000, -0.000000000000000000, 1.000000000000000000 ) ) ;
#5246 = DIRECTION ( 'NONE',  ( -0.000000000000000000, 1.000000000000000000, -0.000000000000000000 ) ) ;
#5247 = DIRECTION ( 'NONE',  ( 1.000000000000000000, 0.000000000000000000, 0.000000000000000000 ) ) ;
#5248 = CARTESIAN_POINT ( 'NONE',  ( 275.0000000000000000, 8.660254037844390851, 145.0000000000000284 ) ) ;
#5249 = DIRECTION ( 'NONE',  ( -0.5000000000000016653, 0.8660254037844378194, 0.000000000000000000 ) ) ;
#5250 = ADVANCED_FACE ( 'NONE', ( #2452 ), #2959, .F. ) ;
#5251 = EDGE_CURVE ( 'NONE', #7046, #6469, #743, .T. ) ;
#5252 = ORIENTED_EDGE ( 'NONE', *, *, #2473, .T. ) ;
#5253 = VERTEX_POINT ( 'NONE', #6369 ) ;
#5254 = CONTEXT_DEPENDENT_SHAPE_REPRESENTATION ( #393, #5471 ) ;
#5255 = CARTESIAN_POINT ( 'NONE',  ( -1.800000000000001155, 0.000000000000000000, -13.29999999999999893 ) ) ;
#5256 = ORIENTED_EDGE ( 'NONE', *, *, #6360, .F. ) ;
#5257 = VECTOR ( 'NONE', #2964, 1000.000000000000000 ) ;
#5258 =( REPRESENTATION_RELATIONSHIP ('NONE','NONE', #5587, #5294 ) REPRESENTATION_RELATIONSHIP_WITH_TRANSFORMATION ( #4800 )SHAPE_REPRESENTATION_RELATIONSHIP( ) );
#5259 = CARTESIAN_POINT ( 'NONE',  ( -4.204114297095464359, 1.660363174096617156, -3.602136431857887011 ) ) ;
#5260 = CIRCLE ( 'NONE', #2020, 13.50000000000000000 ) ;
#5261 = ADVANCED_FACE ( 'NONE', ( #2898 ), #1334, .F. ) ;
#5262 = EDGE_LOOP ( 'NONE', ( #1524, #5713, #6429 ) ) ;
#5263 = FACE_OUTER_BOUND ( 'NONE', #4472, .T. ) ;
#5264 = ADVANCED_FACE ( 'NONE', ( #6962 ), #2933, .F. ) ;
#5265 = DIRECTION ( 'NONE',  ( 1.000000000000000000, 0.000000000000000000, 0.000000000000000000 ) ) ;
#5266 = VECTOR ( 'NONE', #6169, 1000.000000000000000 ) ;
#5267 = ORIENTED_EDGE ( 'NONE', *, *, #3589, .T. ) ;
#5268 = PLANE ( 'NONE',  #6790 ) ;
#5269 = EDGE_CURVE ( 'NONE', #3098, #847, #1269, .T. ) ;
#5270 = EDGE_LOOP ( 'NONE', ( #4022, #2714, #5200, #4034 ) ) ;
#5271 = AXIS2_PLACEMENT_3D ( 'NONE', #6876, #26, #2774 ) ;
#5272 = FACE_OUTER_BOUND ( 'NONE', #4314, .T. ) ;
#5273 = CARTESIAN_POINT ( 'NONE',  ( 4.999999999999999112, 8.660254037844390851, 140.0000000000000000 ) ) ;
#5274 = ITEM_DEFINED_TRANSFORMATION ( 'NONE', 'NONE', #3400,  #1963 ) ;
#5275 = CARTESIAN_POINT ( 'NONE',  ( 2.500000000000000000, 2.357898499370433054, -1.951563910473907981E-15 ) ) ;
#5276 = DIRECTION ( 'NONE',  ( -0.000000000000000000, -0.000000000000000000, 1.000000000000000000 ) ) ;
#5277 = ADVANCED_FACE ( 'NONE', ( #6442 ), #7006, .T. ) ;
#5278 = VERTEX_POINT ( 'NONE', #4040 ) ;
#5279 = LINE ( 'NONE', #7045, #1811 ) ;
#5280 = ORIENTED_EDGE ( 'NONE', *, *, #5940, .F. ) ;
#5281 = ORIENTED_EDGE ( 'NONE', *, *, #3338, .T. ) ;
#5282 = CARTESIAN_POINT ( 'NONE',  ( 315.0000000000000568, 8.660254037844390851, 145.0000000000000284 ) ) ;
#5283 = CARTESIAN_POINT ( 'NONE',  ( 0.1750025118121568690, 4.719839900820621104, -3.469254087858248070 ) ) ;
#5284 = DIRECTION ( 'NONE',  ( 0.000000000000000000, 0.000000000000000000, -1.000000000000000000 ) ) ;
#5285 = CARTESIAN_POINT ( 'NONE',  ( -19.00000000000000000, 0.000000000000000000, 125.0000000000000000 ) ) ;
#5286 = CIRCLE ( 'NONE', #6386, 2.649999999999985700 ) ;
#5287 = PLANE ( 'NONE',  #4589 ) ;
#5288 = ORIENTED_EDGE ( 'NONE', *, *, #1885, .F. ) ;
#5289 = PRODUCT ( 'roller', 'roller', '', ( #6246 ) ) ;
#5290 = AXIS2_PLACEMENT_3D ( 'NONE', #5441, #2113, #6015 ) ;
#5291 = DIRECTION ( 'NONE',  ( -1.000000000000000000, -0.000000000000000000, -0.000000000000000000 ) ) ;
#5292 = ORIENTED_EDGE ( 'NONE', *, *, #7038, .T. ) ;
#5293 = EDGE_CURVE ( 'NONE', #6744, #1972, #5237, .T. ) ;
#5294 = SHAPE_REPRESENTATION ( 'angular contact ball bearing_68_iso_ISO 15 ABB - 1720 - 28,SI,NC,28_68', ( #1963 ), #5797 ) ;
#5295 =( NAMED_UNIT ( * ) PLANE_ANGLE_UNIT ( ) SI_UNIT ( $, .RADIAN. ) );
#5296 = VECTOR ( 'NONE', #2944, 1000.000000000000114 ) ;
#5297 = AXIS2_PLACEMENT_3D ( 'NONE', #7227, #3812, #3852 ) ;
#5298 = CARTESIAN_POINT ( 'NONE',  ( -4.000000000000000000, -2.512220745329312610, -3.469390707569719901 ) ) ;
#5299 = AXIS2_PLACEMENT_3D ( 'NONE', #889, #2594, #6141 ) ;
#5300 = AXIS2_PLACEMENT_3D ( 'NONE', #7130, #3133, #3672 ) ;
#5301 = ORIENTED_EDGE ( 'NONE', *, *, #4235, .F. ) ;
#5302 = PRODUCT_DEFINITION_FORMATION_WITH_SPECIFIED_SOURCE ( 'ANY', '', #4278, .NOT_KNOWN. ) ;
#5303 = CARTESIAN_POINT ( 'NONE',  ( 136.6666666666666288, -20.00000000000000000, 159.8500000000001080 ) ) ;
#5304 = AXIS2_PLACEMENT_3D ( 'NONE', #6005, #3633, #4276 ) ;
#5305 = EDGE_CURVE ( 'NONE', #5197, #1419, #3456, .T. ) ;
#5306 = EDGE_CURVE ( 'NONE', #1084, #6398, #4432, .T. ) ;
#5307 = VERTEX_POINT ( 'NONE', #5310 ) ;
#5308 = ORIENTED_EDGE ( 'NONE', *, *, #6583, .T. ) ;
#5309 =( GEOMETRIC_REPRESENTATION_CONTEXT ( 3 ) GLOBAL_UNCERTAINTY_ASSIGNED_CONTEXT ( ( #3067 ) ) GLOBAL_UNIT_ASSIGNED_CONTEXT ( ( #7253, #6694, #5008 ) ) REPRESENTATION_CONTEXT ( 'NONE', 'WORKASPACE' ) );
#5310 = CARTESIAN_POINT ( 'NONE',  ( 1.999999999999994893, 1.313433692085536476E-15, 10.72499999999999964 ) ) ;
#5311 = DIRECTION ( 'NONE',  ( 1.000000000000000000, 0.000000000000000000, 0.000000000000000000 ) ) ;
#5312 = DIRECTION ( 'NONE',  ( -1.000000000000000000, -0.000000000000000000, -0.000000000000000000 ) ) ;
#5313 = EDGE_CURVE ( 'NONE', #1111, #4048, #3468, .T. ) ;
#5314 = EDGE_CURVE ( 'NONE', #918, #5307, #4180, .T. ) ;
#5315 = CIRCLE ( 'NONE', #4008, 10.00000000000000000 ) ;
#5316 = DIRECTION ( 'NONE',  ( 1.000000000000000000, 0.000000000000000000, 0.000000000000000000 ) ) ;
#5317 = PRESENTATION_LAYER_ASSIGNMENT (  '', '', ( #1839 ) ) ;
#5318 = EDGE_LOOP ( 'NONE', ( #1892, #1011, #4543, #5241 ) ) ;
#5319 = FACE_BOUND ( 'NONE', #6524, .T. ) ;
#5320 = ORIENTED_EDGE ( 'NONE', *, *, #4888, .T. ) ;
#5321 = ORIENTED_EDGE ( 'NONE', *, *, #5466, .F. ) ;
#5322 = CARTESIAN_POINT ( 'NONE',  ( -5.000000000000000888, 8.660254037844390851, 150.0000000000000000 ) ) ;
#5323 = CIRCLE ( 'NONE', #3641, 13.50000000000000000 ) ;
#5324 = DIRECTION ( 'NONE',  ( -0.000000000000000000, 0.000000000000000000, 1.000000000000000000 ) ) ;
#5325 = DIRECTION ( 'NONE',  ( 1.000000000000000000, 0.000000000000000000, 0.000000000000000000 ) ) ;
#5326 = CARTESIAN_POINT ( 'NONE',  ( 386.6666666666666288, -25.00000000000000000, 162.5000000000000853 ) ) ;
#5327 = CARTESIAN_POINT ( 'NONE',  ( 35.00000000000000000, 8.660254037844390851, 140.0000000000000000 ) ) ;
#5328 = DIRECTION ( 'NONE',  ( 0.000000000000000000, -1.000000000000000000, 1.287488025362403787E-15 ) ) ;
#5329 = ORIENTED_EDGE ( 'NONE', *, *, #6128, .T. ) ;
#5330 = ORIENTED_EDGE ( 'NONE', *, *, #652, .F. ) ;
#5331 = CARTESIAN_POINT ( 'NONE',  ( 4.211140560182196957, 2.431303136016536470, -3.745885042887433514 ) ) ;
#5332 = ORIENTED_EDGE ( 'NONE', *, *, #3748, .T. ) ;
#5333 = PRODUCT_DEFINITION_SHAPE ( 'NONE', 'NONE',  #7389 ) ;
#5334 = CARTESIAN_POINT ( 'NONE',  ( -4.000000000000000000, 1.677772373332757194, -3.535253723897187506 ) ) ;
#5335 = ADVANCED_FACE ( 'NONE', ( #6903 ), #1757, .T. ) ;
#5336 = UNCERTAINTY_MEASURE_WITH_UNIT (LENGTH_MEASURE( 1.000000000000000082E-05 ), #6325, 'distance_accuracy_value', 'NONE');
#5337 = AXIS2_PLACEMENT_3D ( 'NONE', #3599, #5903, #3031 ) ;
#5338 = VERTEX_POINT ( 'NONE', #3502 ) ;
#5339 = VERTEX_POINT ( 'NONE', #4643 ) ;
#5340 = FACE_OUTER_BOUND ( 'NONE', #6835, .T. ) ;
#5341 = ORIENTED_EDGE ( 'NONE', *, *, #474, .F. ) ;
#5342 = EDGE_LOOP ( 'NONE', ( #6534, #5281, #6103 ) ) ;
#5343 = ADVANCED_FACE ( 'NONE', ( #5272 ), #6932, .F. ) ;
#5344 = EDGE_CURVE ( 'NONE', #7189, #2910, #5286, .T. ) ;
#5345 = CARTESIAN_POINT ( 'NONE',  ( 5.200000000000002842, 0.000000000000000000, 0.000000000000000000 ) ) ;
#5346 = CONTEXT_DEPENDENT_SHAPE_REPRESENTATION ( #4600, #4023 ) ;
#5347 = FACE_OUTER_BOUND ( 'NONE', #4504, .T. ) ;
#5348 = DIRECTION ( 'NONE',  ( 1.000000000000000000, 0.000000000000000000, 0.000000000000000000 ) ) ;
#5349 = ORIENTED_EDGE ( 'NONE', *, *, #2956, .T. ) ;
#5350 = DIRECTION ( 'NONE',  ( 1.000000000000000000, 0.000000000000000000, 0.000000000000000000 ) ) ;
#5351 = ADVANCED_FACE ( 'NONE', ( #1379 ), #3771, .F. ) ;
#5352 = ORIENTED_EDGE ( 'NONE', *, *, #5997, .F. ) ;
#5353 = EDGE_LOOP ( 'NONE', ( #6795, #3313, #4046, #3879 ) ) ;
#5354 =( REPRESENTATION_RELATIONSHIP ('NONE','NONE', #5587, #5294 ) REPRESENTATION_RELATIONSHIP_WITH_TRANSFORMATION ( #1055 )SHAPE_REPRESENTATION_RELATIONSHIP( ) );
#5355 = DIRECTION ( 'NONE',  ( 0.000000000000000000, -1.000000000000000000, 0.000000000000000000 ) ) ;
#5356 = CARTESIAN_POINT ( 'NONE',  ( 4.000000000000000000, 0.1981133338132474442, 2.382280164152719704E-17 ) ) ;
#5357 = LINE ( 'NONE', #6160, #5889 ) ;
#5358 = DIRECTION ( 'NONE',  ( 0.000000000000000000, 0.000000000000000000, -1.000000000000000000 ) ) ;
#5359 = EDGE_CURVE ( 'NONE', #1168, #6755, #3655, .T. ) ;
#5360 = LINE ( 'NONE', #4196, #2661 ) ;
#5361 = CARTESIAN_POINT ( 'NONE',  ( -5.560781378645575757, 6.809993116116508640E-16, -4.000000000000000000 ) ) ;
#5362 = EDGE_LOOP ( 'NONE', ( #5426, #4001, #835, #179 ) ) ;
#5363 = ITEM_DEFINED_TRANSFORMATION ( 'NONE', 'NONE', #2082,  #1963 ) ;
#5364 = LINE ( 'NONE', #5473, #3124 ) ;
#5365 = ORIENTED_EDGE ( 'NONE', *, *, #4199, .F. ) ;
#5366 = EDGE_CURVE ( 'NONE', #6352, #5434, #820, .T. ) ;
#5367 = DIRECTION ( 'NONE',  ( 1.000000000000000000, 0.000000000000000000, 0.000000000000000000 ) ) ;
#5368 = VERTEX_POINT ( 'NONE', #933 ) ;
#5369 = ORIENTED_EDGE ( 'NONE', *, *, #1230, .F. ) ;
#5370 = DIRECTION ( 'NONE',  ( 0.000000000000000000, 0.000000000000000000, 1.000000000000000000 ) ) ;
#5371 = CARTESIAN_POINT ( 'NONE',  ( 0.000000000000000000, 0.000000000000000000, -121.0000000000000000 ) ) ;
#5372 = LINE ( 'NONE', #257, #642 ) ;
#5373 = DIRECTION ( 'NONE',  ( 1.000000000000000000, 0.000000000000000000, 0.000000000000000000 ) ) ;
#5374 = ORIENTED_EDGE ( 'NONE', *, *, #5680, .T. ) ;
#5375 = DIRECTION ( 'NONE',  ( 1.000000000000000000, 0.000000000000000000, 0.000000000000000000 ) ) ;
#5376 = EDGE_CURVE ( 'NONE', #5585, #586, #1447, .T. ) ;
#5377 = ITEM_DEFINED_TRANSFORMATION ( 'NONE', 'NONE', #5672,  #1963 ) ;
#5378 = CARTESIAN_POINT ( 'NONE',  ( 0.5276280594147412240, -4.314175951381924889, -3.320322319201654881 ) ) ;
#5379 = FACE_BOUND ( 'NONE', #1378, .T. ) ;
#5380 = EDGE_CURVE ( 'NONE', #1873, #4461, #2520, .T. ) ;
#5381 = ORIENTED_EDGE ( 'NONE', *, *, #5306, .T. ) ;
#5382 = AXIS2_PLACEMENT_3D ( 'NONE', #996, #3210, #5512 ) ;
#5383 = FACE_BOUND ( 'NONE', #3621, .T. ) ;
#5384 = CIRCLE ( 'NONE', #6357, 13.50000000000000533 ) ;
#5385 = EDGE_LOOP ( 'NONE', ( #2372, #2337 ) ) ;
#5386 = VERTEX_POINT ( 'NONE', #4856 ) ;
#5387 = CARTESIAN_POINT ( 'NONE',  ( 3.999999999999999112, -0.3979232138631231819, -5.929230630780099908E-17 ) ) ;
#5388 = DIRECTION ( 'NONE',  ( 0.000000000000000000, -0.000000000000000000, -1.000000000000000000 ) ) ;
#5389 = CARTESIAN_POINT ( 'NONE',  ( 4.024499207728657879, 2.323545700935571556, -3.572172305156506411 ) ) ;
#5390 = LINE ( 'NONE', #6490, #6038 ) ;
#5391 = ADVANCED_FACE ( 'NONE', ( #7146 ), #6672, .F. ) ;
#5392 = DIRECTION ( 'NONE',  ( -0.8660254037844377084, -0.5000000000000015543, 0.000000000000000000 ) ) ;
#5393 = DIRECTION ( 'NONE',  ( -1.000000000000000000, 0.000000000000000000, 0.000000000000000000 ) ) ;
#5394 = ORIENTED_EDGE ( 'NONE', *, *, #3853, .F. ) ;
#5395 = VECTOR ( 'NONE', #1135, 1000.000000000000000 ) ;
#5396 = CONTEXT_DEPENDENT_SHAPE_REPRESENTATION ( #6766, #3182 ) ;
#5397 = CARTESIAN_POINT ( 'NONE',  ( 1.800000000000002931, 0.000000000000000000, 0.000000000000000000 ) ) ;
#5398 = EDGE_LOOP ( 'NONE', ( #4948, #4424, #1791, #6603 ) ) ;
#5399 = AXIS2_PLACEMENT_3D ( 'NONE', #4819, #5375, #1415 ) ;
#5400 = DIRECTION ( 'NONE',  ( 0.000000000000000000, 0.000000000000000000, 1.000000000000000000 ) ) ;
#5401 = EDGE_CURVE ( 'NONE', #1772, #6816, #6109, .T. ) ;
#5402 = CARTESIAN_POINT ( 'NONE',  ( 445.0000000000000000, -8.660254037844389075, 145.0000000000000284 ) ) ;
#5403 = ORIENTED_EDGE ( 'NONE', *, *, #2379, .F. ) ;
#5404 = ORIENTED_EDGE ( 'NONE', *, *, #3209, .T. ) ;
#5405 = DIRECTION ( 'NONE',  ( -1.000000000000000000, 0.000000000000000000, -0.000000000000000000 ) ) ;
#5406 = PRODUCT_DEFINITION_SHAPE ( 'NONE', 'NONE',  #7366 ) ;
#5407 = DIRECTION ( 'NONE',  ( 0.000000000000000000, 0.000000000000000000, 1.000000000000000000 ) ) ;
#5408 = AXIS2_PLACEMENT_3D ( 'NONE', #2726, #6152, #5582 ) ;
#5409 = CARTESIAN_POINT ( 'NONE',  ( -1.999999999999996669, 11.05000000000000071, 0.000000000000000000 ) ) ;
#5410 = CYLINDRICAL_SURFACE ( 'NONE', #921, 11.00000000000000000 ) ;
#5411 = ORIENTED_EDGE ( 'NONE', *, *, #2268, .F. ) ;
#5412 = AXIS2_PLACEMENT_3D ( 'NONE', #3840, #2027, #2589 ) ;
#5413 = AXIS2_PLACEMENT_3D ( 'NONE', #7318, #3786, #6086 ) ;
#5414 = AXIS2_PLACEMENT_3D ( 'NONE', #5397, #3708, #324 ) ;
#5415 = DIRECTION ( 'NONE',  ( -0.000000000000000000, -0.000000000000000000, -1.000000000000000000 ) ) ;
#5416 = DIRECTION ( 'NONE',  ( 0.000000000000000000, 0.000000000000000000, -1.000000000000000000 ) ) ;
#5417 = CARTESIAN_POINT ( 'NONE',  ( 355.0000000000000000, -8.660254037844389075, 140.0000000000000000 ) ) ;
#5418 = CARTESIAN_POINT ( 'NONE',  ( 53.33333333333330017, -30.00000000000000355, 162.5000000000000853 ) ) ;
#5419 = ORIENTED_EDGE ( 'NONE', *, *, #7274, .T. ) ;
#5420 = VECTOR ( 'NONE', #3290, 1000.000000000000000 ) ;
#5421 = LINE ( 'NONE', #2043, #4937 ) ;
#5422 =( GEOMETRIC_REPRESENTATION_CONTEXT ( 3 ) GLOBAL_UNCERTAINTY_ASSIGNED_CONTEXT ( ( #4743 ) ) GLOBAL_UNIT_ASSIGNED_CONTEXT ( ( #2506, #6610, #3175 ) ) REPRESENTATION_CONTEXT ( 'NONE', 'WORKASPACE' ) );
#5423 = CIRCLE ( 'NONE', #420, 2.649999999999985700 ) ;
#5424 = ADVANCED_FACE ( 'NONE', ( #971 ), #3228, .T. ) ;
#5425 = ORIENTED_EDGE ( 'NONE', *, *, #4880, .T. ) ;
#5426 = ORIENTED_EDGE ( 'NONE', *, *, #1466, .F. ) ;
#5427 = DIRECTION ( 'NONE',  ( 1.000000000000000000, 0.000000000000000000, -0.000000000000000000 ) ) ;
#5428 = DIRECTION ( 'NONE',  ( -0.000000000000000000, 0.000000000000000000, 1.000000000000000000 ) ) ;
#5429 = CARTESIAN_POINT ( 'NONE',  ( 2.000000000000005329, -3.464101615137751722, 0.000000000000000000 ) ) ;
#5430 = CARTESIAN_POINT ( 'NONE',  ( 53.33333333333330017, -15.00000000000000000, 159.8500000000001080 ) ) ;
#5431 = DIRECTION ( 'NONE',  ( 0.000000000000000000, 0.000000000000000000, 1.000000000000000000 ) ) ;
#5432 = CARTESIAN_POINT ( 'NONE',  ( 0.000000000000000000, 0.000000000000000000, -5.000000000000000000 ) ) ;
#5433 = VECTOR ( 'NONE', #2300, 1000.000000000000000 ) ;
#5434 = VERTEX_POINT ( 'NONE', #422 ) ;
#5435 = EDGE_CURVE ( 'NONE', #2308, #4157, #3188, .T. ) ;
#5436 = LINE ( 'NONE', #3791, #3465 ) ;
#5437 = DIRECTION ( 'NONE',  ( -0.000000000000000000, 1.000000000000000000, -0.000000000000000000 ) ) ;
#5438 = ORIENTED_EDGE ( 'NONE', *, *, #1293, .T. ) ;
#5439 = VECTOR ( 'NONE', #7336, 1000.000000000000000 ) ;
#5440 = AXIS2_PLACEMENT_3D ( 'NONE', #1104, #4471, #4435 ) ;
#5441 = CARTESIAN_POINT ( 'NONE',  ( 386.6666666666666288, -20.00000000000000000, 162.5000000000000853 ) ) ;
#5442 = CARTESIAN_POINT ( 'NONE',  ( 205.0000000000000284, -8.660254037844389075, 145.0000000000000284 ) ) ;
#5443 = ORIENTED_EDGE ( 'NONE', *, *, #70, .T. ) ;
#5444 = EDGE_CURVE ( 'NONE', #3280, #6176, #302, .T. ) ;
#5446 = AXIS2_PLACEMENT_3D ( 'NONE', #4996, #7311, #3240 ) ;
#5445 = DIRECTION ( 'NONE',  ( 0.000000000000000000, 0.000000000000000000, 1.000000000000000000 ) ) ;
#5447 = ORIENTED_EDGE ( 'NONE', *, *, #5401, .F. ) ;
#5448 = DIRECTION ( 'NONE',  ( 0.000000000000000000, 0.000000000000000000, -1.000000000000000000 ) ) ;
#5449 = AXIS2_PLACEMENT_3D ( 'NONE', #4980, #1530, #3149 ) ;
#5450 = CARTESIAN_POINT ( 'NONE',  ( -4.000000000000000000, 2.309401076758498483, -3.433295621305379353 ) ) ;
#5451 = LINE ( 'NONE', #4814, #2227 ) ;
#5452 =( REPRESENTATION_RELATIONSHIP ('NONE','NONE', #5587, #6025 ) REPRESENTATION_RELATIONSHIP_WITH_TRANSFORMATION ( #6518 )SHAPE_REPRESENTATION_RELATIONSHIP( ) );
#5453 = ORIENTED_EDGE ( 'NONE', *, *, #4122, .T. ) ;
#5454 = CARTESIAN_POINT ( 'NONE',  ( 470.0000000000000000, -15.00000000000000000, 180.0000000000000284 ) ) ;
#5455 = FACE_OUTER_BOUND ( 'NONE', #6090, .T. ) ;
#5456 = CARTESIAN_POINT ( 'NONE',  ( 0.000000000000000000, 0.000000000000000000, 140.0000000000000000 ) ) ;
#5457 = DIRECTION ( 'NONE',  ( 6.123233995736766036E-17, -1.000000000000000000, 0.000000000000000000 ) ) ;
#5458 = ORIENTED_EDGE ( 'NONE', *, *, #2864, .T. ) ;
#5459 = CARTESIAN_POINT ( 'NONE',  ( 0.6666666666666658525, -4.233901974057276085, -3.300726591567086476 ) ) ;
#5460 = VERTEX_POINT ( 'NONE', #3723 ) ;
#5461 = VERTEX_POINT ( 'NONE', #3153 ) ;
#5462 = CARTESIAN_POINT ( 'NONE',  ( 2.500000000000000000, -2.357898499370432610, 3.252606517456513302E-15 ) ) ;
#5463 = CARTESIAN_POINT ( 'NONE',  ( 4.000000000000000000, 0.9868501483902631932, -0.09357334158579604100 ) ) ;
#5464 = LINE ( 'NONE', #1508, #1587 ) ;
#5465 = DIRECTION ( 'NONE',  ( -0.000000000000000000, 1.000000000000000000, 0.000000000000000000 ) ) ;
#5466 = EDGE_CURVE ( 'NONE', #3158, #818, #4782, .T. ) ;
#5467 = LINE ( 'NONE', #910, #6390 ) ;
#5468 = LINE ( 'NONE', #2614, #7241 ) ;
#5469 = FACE_OUTER_BOUND ( 'NONE', #5342, .T. ) ;
#5470 = ORIENTED_EDGE ( 'NONE', *, *, #1571, .F. ) ;
#5471 = PRODUCT_DEFINITION_SHAPE ( 'NONE', 'NONE',  #7353 ) ;
#5472 = CYLINDRICAL_SURFACE ( 'NONE', #4071, 2.649999999999985700 ) ;
#5473 = CARTESIAN_POINT ( 'NONE',  ( -10.00000000000000000, 0.000000000000000000, 140.0000000000000000 ) ) ;
#5474 = ORIENTED_EDGE ( 'NONE', *, *, #1014, .T. ) ;
#5475 = CARTESIAN_POINT ( 'NONE',  ( -5.000000000000000888, 8.660254037844390851, 150.0000000000000000 ) ) ;
#5476 = EDGE_CURVE ( 'NONE', #2468, #1612, #3687, .T. ) ;
#5477 = FILL_AREA_STYLE ('',( #3675 ) ) ;
#5478 = DIRECTION ( 'NONE',  ( 0.000000000000000000, -0.000000000000000000, 1.000000000000000000 ) ) ;
#5479 = ADVANCED_FACE ( 'NONE', ( #5529 ), #1708, .F. ) ;
#5480 = CARTESIAN_POINT ( 'NONE',  ( 2.000000000000001776, 0.000000000000000000, -13.29999999999999893 ) ) ;
#5481 = ORIENTED_EDGE ( 'NONE', *, *, #4837, .F. ) ;
#5482 = DIRECTION ( 'NONE',  ( 1.000000000000000000, 0.000000000000000000, 0.000000000000000000 ) ) ;
#5483 = VERTEX_POINT ( 'NONE', #5694 ) ;
#5484 = DIRECTION ( 'NONE',  ( 0.000000000000000000, 0.000000000000000000, 1.000000000000000000 ) ) ;
#5485 = EDGE_CURVE ( 'NONE', #1538, #732, #3429, .T. ) ;
#5486 = CYLINDRICAL_SURFACE ( 'NONE', #7097, 13.50000000000000000 ) ;
#5487 = FACE_OUTER_BOUND ( 'NONE', #2919, .T. ) ;
#5488 = ORIENTED_EDGE ( 'NONE', *, *, #5376, .F. ) ;
#5489 = CARTESIAN_POINT ( 'NONE',  ( -31.74999999999995737, 0.000000000000000000, 4.250000000000000000 ) ) ;
#5490 = FACE_OUTER_BOUND ( 'NONE', #518, .T. ) ;
#5491 = DIRECTION ( 'NONE',  ( -0.000000000000000000, 1.000000000000000000, -0.000000000000000000 ) ) ;
#5492 = CARTESIAN_POINT ( 'NONE',  ( 40.00000000000000000, 0.000000000000000000, 0.000000000000000000 ) ) ;
#5493 = APPLICATION_CONTEXT ( 'automotive_design' ) ;
#5494 = ADVANCED_FACE ( 'NONE', ( #3968 ), #1570, .F. ) ;
#5495 = EDGE_LOOP ( 'NONE', ( #426, #252, #124, #3900 ) ) ;
#5496 = DIRECTION ( 'NONE',  ( -0.8660254037844373753, 0.5000000000000021094, 0.000000000000000000 ) ) ;
#5497 = AXIS2_PLACEMENT_3D ( 'NONE', #3818, #350, #313 ) ;
#5498 = ORIENTED_EDGE ( 'NONE', *, *, #2365, .T. ) ;
#5499 = VERTEX_POINT ( 'NONE', #6745 ) ;
#5500 = LINE ( 'NONE', #4906, #6233 ) ;
#5501 = CARTESIAN_POINT ( 'NONE',  ( 0.000000000000000000, 0.000000000000000000, -125.0000000000000000 ) ) ;
#5502 = ITEM_DEFINED_TRANSFORMATION ( 'NONE', 'NONE', #1252,  #1963 ) ;
#5503 = DIRECTION ( 'NONE',  ( 0.000000000000000000, -1.000000000000000000, 0.000000000000000000 ) ) ;
#5504 = DIRECTION ( 'NONE',  ( -1.000000000000000000, -0.000000000000000000, -0.000000000000000000 ) ) ;
#5505 = CIRCLE ( 'NONE', #5987, 2.649999999999985700 ) ;
#5506 = FACE_OUTER_BOUND ( 'NONE', #2048, .T. ) ;
#5507 = CARTESIAN_POINT ( 'NONE',  ( 136.6666666666666288, -25.00000000000000000, -162.5000000000000853 ) ) ;
#5508 = ORIENTED_EDGE ( 'NONE', *, *, #6139, .T. ) ;
#5509 = AXIS2_PLACEMENT_3D ( 'NONE', #5885, #6422, #2975 ) ;
#5510 = CARTESIAN_POINT ( 'NONE',  ( 0.000000000000000000, 1.438959988998140160E-15, -11.75000000000000000 ) ) ;
#5511 = DIRECTION ( 'NONE',  ( 0.000000000000000000, 0.000000000000000000, 1.000000000000000000 ) ) ;
#5512 = DIRECTION ( 'NONE',  ( 0.000000000000000000, 0.000000000000000000, 1.000000000000000000 ) ) ;
#5513 =( NAMED_UNIT ( * ) SI_UNIT ( $, .STERADIAN. ) SOLID_ANGLE_UNIT ( ) );
#5514 = CARTESIAN_POINT ( 'NONE',  ( 1.799999999999996048, 0.000000000000000000, -9.999999999999994671 ) ) ;
#5515 = B_SPLINE_CURVE_WITH_KNOTS ( 'NONE', 3,
 ( #2462, #5929, #4727, #6487, #1867 ),
 .UNSPECIFIED., .F., .F.,
 ( 4, 1, 4 ),
 ( 0.000000000000000000, 0.002309401076758505790, 0.004618802153517011580 ),
 .UNSPECIFIED. ) ;
#5516 = LINE ( 'NONE', #7100, #1166 ) ;
#5517 = VECTOR ( 'NONE', #7186, 1000.000000000000000 ) ;
#5518 = EDGE_LOOP ( 'NONE', ( #914, #1292, #952, #2645 ) ) ;
#5519 = EDGE_LOOP ( 'NONE', ( #2366, #1615 ) ) ;
#5520 = EDGE_CURVE ( 'NONE', #1382, #5585, #5058, .T. ) ;
#5521 = DIRECTION ( 'NONE',  ( 1.000000000000000000, 0.000000000000000000, 0.000000000000000000 ) ) ;
#5522 = ORIENTED_EDGE ( 'NONE', *, *, #6846, .T. ) ;
#5523 = DIRECTION ( 'NONE',  ( -0.000000000000000000, 1.000000000000000000, -0.000000000000000000 ) ) ;
#5524 = AXIS2_PLACEMENT_3D ( 'NONE', #5819, #692, #4762 ) ;
#5525 = CARTESIAN_POINT ( 'NONE',  ( -1.999999999999999556, 3.464101615137754830, -3.142992957459232795 ) ) ;
#5526 = DIRECTION ( 'NONE',  ( -1.000000000000000000, 0.000000000000000000, 0.000000000000000000 ) ) ;
#5527 = ORIENTED_EDGE ( 'NONE', *, *, #2199, .T. ) ;
#5528 = ADVANCED_FACE ( 'NONE', ( #4452 ), #7333, .F. ) ;
#5529 = FACE_OUTER_BOUND ( 'NONE', #4778, .T. ) ;
#5530 = PRESENTATION_LAYER_ASSIGNMENT (  '', '', ( #6746 ) ) ;
#5531 = CONTEXT_DEPENDENT_SHAPE_REPRESENTATION ( #5748, #2334 ) ;
#5532 = CARTESIAN_POINT ( 'NONE',  ( 53.33333333333330017, -20.00000000000000000, -162.5000000000000853 ) ) ;
#5533 = PLANE ( 'NONE',  #6046 ) ;
#5534 = DIRECTION ( 'NONE',  ( 0.000000000000000000, 0.000000000000000000, 1.000000000000000000 ) ) ;
#5535 = ORIENTED_EDGE ( 'NONE', *, *, #6699, .T. ) ;
#5536 = CARTESIAN_POINT ( 'NONE',  ( 4.999999999999999112, 8.660254037844390851, 150.0000000000000000 ) ) ;
#5537 = PRODUCT_DEFINITION_SHAPE ( 'NONE', 'NONE',  #7371 ) ;
#5538 = MECHANICAL_DESIGN_GEOMETRIC_PRESENTATION_REPRESENTATION (  '', ( #3378 ), #169 ) ;
#5539 = PRODUCT_DEFINITION_FORMATION_WITH_SPECIFIED_SOURCE ( 'ANY', '', #5289, .NOT_KNOWN. ) ;
#5540 = VECTOR ( 'NONE', #3291, 1000.000000000000000 ) ;
#5541 = CIRCLE ( 'NONE', #1008, 10.00000000000000000 ) ;
#5542 = VECTOR ( 'NONE', #3102, 1000.000000000000000 ) ;
#5543 = VERTEX_POINT ( 'NONE', #3848 ) ;
#5544 = ORIENTED_EDGE ( 'NONE', *, *, #329, .F. ) ;
#5545 = EDGE_CURVE ( 'NONE', #6988, #6714, #2796, .T. ) ;
#5546 = CARTESIAN_POINT ( 'NONE',  ( 4.000000000000000000, 0.000000000000000000, 0.000000000000000000 ) ) ;
#5547 = DIRECTION ( 'NONE',  ( -0.000000000000000000, 0.000000000000000000, 1.000000000000000000 ) ) ;
#5548 = ITEM_DEFINED_TRANSFORMATION ( 'NONE', 'NONE', #4097,  #1963 ) ;
#5549 = DIRECTION ( 'NONE',  ( 0.000000000000000000, -1.000000000000000000, 0.000000000000000000 ) ) ;
#5550 = LINE ( 'NONE', #3863, #2676 ) ;
#5551 = VECTOR ( 'NONE', #5820, 1000.000000000000000 ) ;
#5552 = AXIS2_PLACEMENT_3D ( 'NONE', #7319, #2318, #585 ) ;
#5553 = AXIS2_PLACEMENT_3D ( 'NONE', #7264, #3720, #3844 ) ;
#5554 = PRODUCT_DEFINITION_CONTEXT ( 'detailed design', #4252, 'design' ) ;
#5555 = CARTESIAN_POINT ( 'NONE',  ( 386.6666666666666288, -20.00000000000000000, 159.8500000000001080 ) ) ;
#5556 = VERTEX_POINT ( 'NONE', #2196 ) ;
#5557 = AXIS2_PLACEMENT_3D ( 'NONE', #2253, #4550, #3986 ) ;
#5558 = MECHANICAL_DESIGN_GEOMETRIC_PRESENTATION_REPRESENTATION (  '', ( #6516 ), #2540 ) ;
#5559 = CARTESIAN_POINT ( 'NONE',  ( -5.000000000000000888, 8.660254037844390851, -150.0000000000000000 ) ) ;
#5560 = CARTESIAN_POINT ( 'NONE',  ( -2.500000000000000888, 0.000000000000000000, -4.974599999999998801 ) ) ;
#5561 = CARTESIAN_POINT ( 'NONE',  ( -1.312671235360383548, -3.860931062424228788, -0.05923475698271369466 ) ) ;
#5562 = FACE_OUTER_BOUND ( 'NONE', #1662, .T. ) ;
#5563 = AXIS2_PLACEMENT_3D ( 'NONE', #6632, #2522, #2601 ) ;
#5564 = DIRECTION ( 'NONE',  ( 0.000000000000000000, -1.000000000000000000, 1.287488025362403787E-15 ) ) ;
#5565 = ORIENTED_EDGE ( 'NONE', *, *, #4916, .T. ) ;
#5566 = ORIENTED_EDGE ( 'NONE', *, *, #7141, .F. ) ;
#5567 = DIRECTION ( 'NONE',  ( 0.000000000000000000, 0.000000000000000000, -1.000000000000000000 ) ) ;
#5568 = VECTOR ( 'NONE', #188, 1000.000000000000000 ) ;
#5569 = EDGE_LOOP ( 'NONE', ( #1504, #3610, #5594, #4362 ) ) ;
#5570 = AXIS2_PLACEMENT_3D ( 'NONE', #4248, #6541, #328 ) ;
#5571 = FACE_OUTER_BOUND ( 'NONE', #4638, .T. ) ;
#5572 = ADVANCED_FACE ( 'NONE', ( #5577, #6301, #4983, #6254, #1015, #1121, #5100, #3394, #6188, #5131, #3274 ), #2159, .T. ) ;
#5573 = DIRECTION ( 'NONE',  ( 0.000000000000000000, 0.000000000000000000, 1.000000000000000000 ) ) ;
#5574 = DIRECTION ( 'NONE',  ( 0.000000000000000000, 0.000000000000000000, 1.000000000000000000 ) ) ;
#5575 = AXIS2_PLACEMENT_3D ( 'NONE', #4612, #2866, #3469 ) ;
#5576 = ORIENTED_EDGE ( 'NONE', *, *, #5758, .F. ) ;
#5577 = FACE_BOUND ( 'NONE', #348, .T. ) ;
#5578 = FACE_OUTER_BOUND ( 'NONE', #2948, .T. ) ;
#5579 = LINE ( 'NONE', #572, #2686 ) ;
#5580 = DIRECTION ( 'NONE',  ( 0.000000000000000000, 0.000000000000000000, -1.000000000000000000 ) ) ;
#5581 = EDGE_LOOP ( 'NONE', ( #3980, #5075, #92, #4031 ) ) ;
#5582 = DIRECTION ( 'NONE',  ( 0.000000000000000000, 0.000000000000000000, -1.000000000000000000 ) ) ;
#5583 = EDGE_CURVE ( 'NONE', #853, #1606, #5669, .T. ) ;
#5584 = ORIENTED_EDGE ( 'NONE', *, *, #2954, .F. ) ;
#5585 = VERTEX_POINT ( 'NONE', #2720 ) ;
#5586 = DIRECTION ( 'NONE',  ( 0.000000000000000000, 0.000000000000000000, 1.000000000000000000 ) ) ;
#5587 = SHAPE_REPRESENTATION ( 'MAS-189', ( #1130, #6622, #2082, #4366, #893, #6024, #552, #1472, #3379, #5297, #6293, #2061, #2203, #186, #4341, #6643, #3760, #3022, #3140, #1252, #6813, #7215, #4097, #3612, #6978, #874, #6047, #6400, #5093, #3990, #5073, #1492, #5664, #1815, #5687, #3732, #6270, #2409, #2999, #1123, #2433, #2802, #756, #6996, #1712, #6870, #5902, #2663, #3400, #411, #4590, #173, #1351, #2888, #4954, #4102, #1601, #5672, #3252, #6030, #4217, #5412, #6279, #6153, #6627, #2187, #56, #4595, #2419, #1006, #7222, #5785 ), #4351 ) ;
#5588 = FACE_OUTER_BOUND ( 'NONE', #4266, .T. ) ;
#5589 = CARTESIAN_POINT ( 'NONE',  ( 2.345747346278113987, -3.264484291692503870, -0.01223254789874484924 ) ) ;
#5590 = CARTESIAN_POINT ( 'NONE',  ( 0.000000000000000000, -1.178949249685213863, 2.042000000000002924 ) ) ;
#5591 = CARTESIAN_POINT ( 'NONE',  ( 205.0000000000000284, 8.660254037844390851, 145.0000000000000284 ) ) ;
#5592 = DIRECTION ( 'NONE',  ( -1.000000000000000000, 0.000000000000000000, 0.000000000000000000 ) ) ;
#5593 = EDGE_CURVE ( 'NONE', #6342, #7102, #269, .T. ) ;
#5594 = ORIENTED_EDGE ( 'NONE', *, *, #521, .T. ) ;
#5595 = CARTESIAN_POINT ( 'NONE',  ( 136.6666666666666288, -15.00000000000000000, 162.5000000000000853 ) ) ;
#5596 = EDGE_CURVE ( 'NONE', #1179, #4485, #2123, .T. ) ;
#5597 = CARTESIAN_POINT ( 'NONE',  ( 0.000000000000000000, 0.000000000000000000, 0.000000000000000000 ) ) ;
#5598 = CARTESIAN_POINT ( 'NONE',  ( -1.144235203016679359, -3.958177651039096911, -0.09382832055446428676 ) ) ;
#5599 =( NAMED_UNIT ( * ) PLANE_ANGLE_UNIT ( ) SI_UNIT ( $, .RADIAN. ) );
#5600 = SHAPE_REPRESENTATION_RELATIONSHIP ( 'NONE' , 'NONE' ,  #4771, #2710 ) ;
#5601 = CARTESIAN_POINT ( 'NONE',  ( 2.500000000000000000, 0.000000000000000000, 0.000000000000000000 ) ) ;
#5602 = ORIENTED_EDGE ( 'NONE', *, *, #5583, .T. ) ;
#5603 = LINE ( 'NONE', #5621, #6578 ) ;
#5604 = ORIENTED_EDGE ( 'NONE', *, *, #7031, .T. ) ;
#5605 = DIRECTION ( 'NONE',  ( 1.000000000000000000, 0.000000000000000000, 0.000000000000000000 ) ) ;
#5606 = ORIENTED_EDGE ( 'NONE', *, *, #3273, .T. ) ;
#5607 =( REPRESENTATION_RELATIONSHIP ('NONE','NONE', #5587, #1193 ) REPRESENTATION_RELATIONSHIP_WITH_TRANSFORMATION ( #4894 )SHAPE_REPRESENTATION_RELATIONSHIP( ) );
#5608 = DIRECTION ( 'NONE',  ( -0.000000000000000000, 0.000000000000000000, 1.000000000000000000 ) ) ;
#5609 = EDGE_CURVE ( 'NONE', #3098, #647, #3481, .T. ) ;
#5610 = PLANE ( 'NONE',  #4474 ) ;
#5611 = CARTESIAN_POINT ( 'NONE',  ( 10.00000000000000000, 1.224646799147353256E-15, -140.0000000000000000 ) ) ;
#5612 = ORIENTED_EDGE ( 'NONE', *, *, #6730, .F. ) ;
#5613 = DIRECTION ( 'NONE',  ( -0.000000000000000000, -0.000000000000000000, 1.000000000000000000 ) ) ;
#5614 = CARTESIAN_POINT ( 'NONE',  ( 75.00000000000001421, -8.660254037844389075, 145.0000000000000284 ) ) ;
#5615 = DIRECTION ( 'NONE',  ( 1.000000000000000000, 0.000000000000000000, 0.000000000000000000 ) ) ;
#5616 = EDGE_LOOP ( 'NONE', ( #2239, #4070, #4919, #4903 ) ) ;
#5617 = FACE_OUTER_BOUND ( 'NONE', #1575, .T. ) ;
#5618 = VERTEX_POINT ( 'NONE', #5057 ) ;
#5619 = EDGE_CURVE ( 'NONE', #3869, #1933, #2683, .T. ) ;
#5620 = ORIENTED_EDGE ( 'NONE', *, *, #1159, .T. ) ;
#5621 = CARTESIAN_POINT ( 'NONE',  ( 275.0000000000000000, -8.660254037844389075, 139.9990000000000236 ) ) ;
#5622 = CARTESIAN_POINT ( 'NONE',  ( 1.999999999999998668, 1.249139735130300365E-15, 10.20000000000000107 ) ) ;
#5623 = CONTEXT_DEPENDENT_SHAPE_REPRESENTATION ( #6137, #1408 ) ;
#5624 = CARTESIAN_POINT ( 'NONE',  ( 4.000000000000000000, 2.309401076758497151, -3.433295621305379353 ) ) ;
#5625 = CARTESIAN_POINT ( 'NONE',  ( 275.0000000000000000, 8.660254037844390851, 145.0000000000000284 ) ) ;
#5626 = DIRECTION ( 'NONE',  ( 0.000000000000000000, 0.000000000000000000, -1.000000000000000000 ) ) ;
#5627 = CYLINDRICAL_SURFACE ( 'NONE', #421, 2.649999999999985700 ) ;
#5628 = AXIS2_PLACEMENT_3D ( 'NONE', #272, #4995, #1458 ) ;
#5629 = ORIENTED_EDGE ( 'NONE', *, *, #4411, .T. ) ;
#5630 = DIRECTION ( 'NONE',  ( 0.000000000000000000, -0.000000000000000000, 1.000000000000000000 ) ) ;
#5631 = CYLINDRICAL_SURFACE ( 'NONE', #4844, 2.649999999999985700 ) ;
#5632 = CARTESIAN_POINT ( 'NONE',  ( 315.0000000000000568, 8.660254037844390851, 139.9990000000000236 ) ) ;
#5633 = FACE_OUTER_BOUND ( 'NONE', #6269, .T. ) ;
#5634 = AXIS2_PLACEMENT_3D ( 'NONE', #1913, #3070, #4436 ) ;
#5635 = EDGE_CURVE ( 'NONE', #977, #2423, #6367, .T. ) ;
#5636 = ADVANCED_FACE ( 'NONE', ( #1645, #6219 ), #1086, .T. ) ;
#5637 = LINE ( 'NONE', #5086, #4096 ) ;
#5638 = EDGE_LOOP ( 'NONE', ( #5158, #1718, #5795, #3736, #773 ) ) ;
#5639 = VERTEX_POINT ( 'NONE', #4242 ) ;
#5640 = SHAPE_DEFINITION_REPRESENTATION ( #4412, #5023 ) ;
#5641 = ORIENTED_EDGE ( 'NONE', *, *, #4935, .F. ) ;
#5642 = ADVANCED_FACE ( 'NONE', ( #5263 ), #6361, .F. ) ;
#5643 = CARTESIAN_POINT ( 'NONE',  ( 0.000000000000000000, 0.000000000000000000, -121.0000000000000000 ) ) ;
#5644 = EDGE_CURVE ( 'NONE', #5278, #4072, #6764, .T. ) ;
#5645 = CARTESIAN_POINT ( 'NONE',  ( 4.211140560182196957, -2.431303136016555122, -3.745885042887436622 ) ) ;
#5646 = VERTEX_POINT ( 'NONE', #5835 ) ;
#5647 = DIRECTION ( 'NONE',  ( -0.000000000000000000, -0.000000000000000000, 1.000000000000000000 ) ) ;
#5648 = VECTOR ( 'NONE', #3829, 1000.000000000000000 ) ;
#5649 = CARTESIAN_POINT ( 'NONE',  ( 4.000000000000000000, 2.512223110932545023, -3.469391141908803711 ) ) ;
#5650 = VECTOR ( 'NONE', #2598, 1000.000000000000000 ) ;
#5651 = DIRECTION ( 'NONE',  ( 0.000000000000000000, 0.000000000000000000, -1.000000000000000000 ) ) ;
#5652 = DIRECTION ( 'NONE',  ( -1.000000000000000000, -6.123233995736766036E-17, -6.123233995736764803E-17 ) ) ;
#5653 = EDGE_LOOP ( 'NONE', ( #6688, #3181 ) ) ;
#5654 = LINE ( 'NONE', #2801, #2669 ) ;
#5655 = ORIENTED_EDGE ( 'NONE', *, *, #5982, .T. ) ;
#5656 = VERTEX_POINT ( 'NONE', #7132 ) ;
#5657 = DIRECTION ( 'NONE',  ( 0.000000000000000000, 0.000000000000000000, 1.000000000000000000 ) ) ;
#5658 = DIRECTION ( 'NONE',  ( -1.000000000000000000, 0.000000000000000000, -0.000000000000000000 ) ) ;
#5659 = ITEM_DEFINED_TRANSFORMATION ( 'NONE', 'NONE', #3612,  #1963 ) ;
#5660 = CARTESIAN_POINT ( 'NONE',  ( 325.0000000000000000, -8.660254037844389075, 140.0000000000000000 ) ) ;
#5661 = LINE ( 'NONE', #1689, #1143 ) ;
#5662 = VECTOR ( 'NONE', #5934, 1000.000000000000000 ) ;
#5663 = EDGE_LOOP ( 'NONE', ( #4469, #2689, #2256, #34, #4790, #6803, #3912 ) ) ;
#5664 = AXIS2_PLACEMENT_3D ( 'NONE', #2759, #3431, #3931 ) ;
#5665 = DIRECTION ( 'NONE',  ( -0.000000000000000000, 1.000000000000000000, -0.000000000000000000 ) ) ;
#5666 = ADVANCED_FACE ( 'NONE', ( #5975 ), #3491, .T. ) ;
#5667 = VECTOR ( 'NONE', #1906, 1000.000000000000000 ) ;
#5668 = ORIENTED_EDGE ( 'NONE', *, *, #5000, .T. ) ;
#5669 = CIRCLE ( 'NONE', #1806, 2.500000000000000888 ) ;
#5670 = CARTESIAN_POINT ( 'NONE',  ( 0.000000000000000000, 0.000000000000000000, 125.0000000000000000 ) ) ;
#5671 = CARTESIAN_POINT ( 'NONE',  ( 5.000000000000000888, 4.250000000000000000, 0.000000000000000000 ) ) ;
#5672 = AXIS2_PLACEMENT_3D ( 'NONE', #2629, #4444, #3218 ) ;
#5673 = CIRCLE ( 'NONE', #4218, 2.649999999999985700 ) ;
#5674 = CARTESIAN_POINT ( 'NONE',  ( 4.024499207728657879, -2.323545700935587988, -3.572172305156509964 ) ) ;
#5675 = FACE_OUTER_BOUND ( 'NONE', #715, .T. ) ;
#5676 = MANIFOLD_SOLID_BREP ( 'Mirror1', #6149 ) ;
#5677 =( NAMED_UNIT ( * ) PLANE_ANGLE_UNIT ( ) SI_UNIT ( $, .RADIAN. ) );
#5678 = CIRCLE ( 'NONE', #2793, 2.100000000000000089 ) ;
#5679 = PRESENTATION_LAYER_ASSIGNMENT (  '', '', ( #547 ) ) ;
#5680 = EDGE_CURVE ( 'NONE', #1772, #432, #1643, .T. ) ;
#5681 = ORIENTED_EDGE ( 'NONE', *, *, #6441, .T. ) ;
#5682 = ORIENTED_EDGE ( 'NONE', *, *, #6205, .T. ) ;
#5683 = EDGE_CURVE ( 'NONE', #2446, #586, #6802, .T. ) ;
#5684 = DIRECTION ( 'NONE',  ( -1.000000000000000000, 0.000000000000000000, 0.000000000000000000 ) ) ;
#5685 = ORIENTED_EDGE ( 'NONE', *, *, #1527, .F. ) ;
#5686 = CIRCLE ( 'NONE', #2432, 10.72500000000000142 ) ;
#5687 = AXIS2_PLACEMENT_3D ( 'NONE', #4567, #6191, #5060 ) ;
#5688 = CYLINDRICAL_SURFACE ( 'NONE', #3122, 2.649999999999985700 ) ;
#5689 = CARTESIAN_POINT ( 'NONE',  ( 0.3461262719736147297, -4.658553426539303821, -3.671615880910379381 ) ) ;
#5690 = EDGE_CURVE ( 'NONE', #7294, #847, #3534, .T. ) ;
#5691 = VECTOR ( 'NONE', #4810, 1000.000000000000000 ) ;
#5692 = ORIENTED_EDGE ( 'NONE', *, *, #3639, .T. ) ;
#5693 = AXIS2_PLACEMENT_3D ( 'NONE', #6727, #6840, #1664 ) ;
#5694 = CARTESIAN_POINT ( 'NONE',  ( 365.0000000000000000, 8.660254037844390851, 145.0000000000000284 ) ) ;
#5695 = EDGE_CURVE ( 'NONE', #2157, #3722, #4632, .T. ) ;
#5696 = CARTESIAN_POINT ( 'NONE',  ( 0.2277608394786177770, 0.000000000000000000, 0.000000000000000000 ) ) ;
#5697 = CARTESIAN_POINT ( 'NONE',  ( 160.0000000000000000, 0.000000000000000000, 0.000000000000000000 ) ) ;
#5698 = AXIS2_PLACEMENT_3D ( 'NONE', #1543, #434, #3404 ) ;
#5699 = ORIENTED_EDGE ( 'NONE', *, *, #5825, .F. ) ;
#5700 = PLANE ( 'NONE',  #4110 ) ;
#5701 = MANIFOLD_SOLID_BREP ( 'Hex', #1931 ) ;
#5702 = ORIENTED_EDGE ( 'NONE', *, *, #5583, .F. ) ;
#5703 = DIRECTION ( 'NONE',  ( -0.000000000000000000, 0.000000000000000000, -1.000000000000000000 ) ) ;
#5704 = VECTOR ( 'NONE', #2790, 1000.000000000000000 ) ;
#5705 = CARTESIAN_POINT ( 'NONE',  ( -5.384454397937118664, 6.702023979852544604E-16, -5.000000000000000000 ) ) ;
#5706 = ITEM_DEFINED_TRANSFORMATION ( 'NONE', 'NONE', #6870,  #1963 ) ;
#5707 = FACE_OUTER_BOUND ( 'NONE', #6116, .T. ) ;
#5708 = LINE ( 'NONE', #1205, #1368 ) ;
#5709 = EDGE_LOOP ( 'NONE', ( #4593, #3651, #938, #3435, #5964, #1093 ) ) ;
#5710 = FACE_OUTER_BOUND ( 'NONE', #679, .T. ) ;
#5711 = VECTOR ( 'NONE', #290, 1000.000000000000000 ) ;
#5712 = EDGE_CURVE ( 'NONE', #6275, #1344, #6202, .T. ) ;
#5713 = ORIENTED_EDGE ( 'NONE', *, *, #5184, .T. ) ;
#5714 = CARTESIAN_POINT ( 'NONE',  ( -5.000000000000000888, -8.660254037844389075, 139.9990000000000236 ) ) ;
#5715 = DIRECTION ( 'NONE',  ( 0.000000000000000000, -0.4999999999999993894, 0.8660254037844389297 ) ) ;
#5716 = CARTESIAN_POINT ( 'NONE',  ( 0.000000000000000000, 8.660254037844390851, 140.0000000000000000 ) ) ;
#5717 = FACE_BOUND ( 'NONE', #5879, .T. ) ;
#5718 =( NAMED_UNIT ( * ) SI_UNIT ( $, .STERADIAN. ) SOLID_ANGLE_UNIT ( ) );
#5719 = ORIENTED_EDGE ( 'NONE', *, *, #6554, .F. ) ;
#5720 = APPLICATION_PROTOCOL_DEFINITION ( 'draft international standard', 'automotive_design', 1998, #1200 ) ;
#5721 = ORIENTED_EDGE ( 'NONE', *, *, #3744, .T. ) ;
#5722 = EDGE_CURVE ( 'NONE', #3854, #5339, #4671, .T. ) ;
#5723 = DIRECTION ( 'NONE',  ( 0.000000000000000000, 0.000000000000000000, 1.000000000000000000 ) ) ;
#5724 = EDGE_CURVE ( 'NONE', #7102, #6342, #2387, .T. ) ;
#5725 = EDGE_LOOP ( 'NONE', ( #135, #6705, #664, #1061 ) ) ;
#5726 = DIRECTION ( 'NONE',  ( 1.000000000000000000, 0.000000000000000000, 0.000000000000000000 ) ) ;
#5727 = EDGE_LOOP ( 'NONE', ( #5028, #6889, #6077, #6935 ) ) ;
#5728 = DIRECTION ( 'NONE',  ( 0.000000000000000000, 0.000000000000000000, 1.000000000000000000 ) ) ;
#5729 = DIRECTION ( 'NONE',  ( -1.000000000000000000, -0.000000000000000000, -0.000000000000000000 ) ) ;
#5730 = ADVANCED_FACE ( 'NONE', ( #5562 ), #6772, .F. ) ;
#5731 = DIRECTION ( 'NONE',  ( 1.000000000000000000, 0.000000000000000000, 0.000000000000000000 ) ) ;
#5732 = VERTEX_POINT ( 'NONE', #482 ) ;
#5733 = CARTESIAN_POINT ( 'NONE',  ( 395.0000000000000000, 8.660254037844390851, 140.0000000000000000 ) ) ;
#5734 = ORIENTED_EDGE ( 'NONE', *, *, #1189, .T. ) ;
#5735 = CARTESIAN_POINT ( 'NONE',  ( 5.200000000000002842, 3.061616997868384127E-16, -2.500000000000000888 ) ) ;
#5736 = DIRECTION ( 'NONE',  ( 0.000000000000000000, 0.000000000000000000, -1.000000000000000000 ) ) ;
#5737 = CARTESIAN_POINT ( 'NONE',  ( 136.6666666666666288, -20.00000000000000000, -159.8500000000001080 ) ) ;
#5738 = DIRECTION ( 'NONE',  ( 0.000000000000000000, 0.000000000000000000, -1.000000000000000000 ) ) ;
#5739 = EDGE_CURVE ( 'NONE', #4072, #1932, #5755, .T. ) ;
#5740 = ORIENTED_EDGE ( 'NONE', *, *, #7320, .F. ) ;
#5741 = CYLINDRICAL_SURFACE ( 'NONE', #3623, 2.649999999999985700 ) ;
#5742 = ORIENTED_EDGE ( 'NONE', *, *, #6559, .F. ) ;
#5743 = FACE_OUTER_BOUND ( 'NONE', #3625, .T. ) ;
#5744 = CARTESIAN_POINT ( 'NONE',  ( 0.000000000000000000, 0.000000000000000000, -125.0000000000000000 ) ) ;
#5745 = LINE ( 'NONE', #619, #3347 ) ;
#5746 = CARTESIAN_POINT ( 'NONE',  ( 0.000000000000000000, 2.357898499370433054, -1.951563910473907981E-15 ) ) ;
#5747 = DIRECTION ( 'NONE',  ( -0.000000000000000000, 1.000000000000000000, -0.000000000000000000 ) ) ;
#5748 =( REPRESENTATION_RELATIONSHIP ('NONE','NONE', #5587, #5294 ) REPRESENTATION_RELATIONSHIP_WITH_TRANSFORMATION ( #4985 )SHAPE_REPRESENTATION_RELATIONSHIP( ) );
#5749 = ORIENTED_EDGE ( 'NONE', *, *, #3432, .F. ) ;
#5750 = APPLICATION_PROTOCOL_DEFINITION ( 'draft international standard', 'automotive_design', 1998, #5793 ) ;
#5751 = ORIENTED_EDGE ( 'NONE', *, *, #6689, .T. ) ;
#5752 = PRODUCT_DEFINITION_SHAPE ( 'NONE', 'NONE',  #7403 ) ;
#5753 = SHAPE_REPRESENTATION_RELATIONSHIP ( 'NONE' , 'NONE' ,  #1193, #1370 ) ;
#5754 = ADVANCED_BREP_SHAPE_REPRESENTATION ( '', ( #3189, #1963 ), #5422 ) ;
#5755 = CIRCLE ( 'NONE', #2158, 4.000000000000000000 ) ;
#5756 = AXIS2_PLACEMENT_3D ( 'NONE', #6841, #1737, #3951 ) ;
#5757 = PLANE ( 'NONE',  #5337 ) ;
#5758 = EDGE_CURVE ( 'NONE', #6697, #4492, #6655, .T. ) ;
#5759 = ORIENTED_EDGE ( 'NONE', *, *, #1919, .F. ) ;
#5760 = CARTESIAN_POINT ( 'NONE',  ( -2.171643655288372443, 3.365003104552320767, 2.541098841762897165E-18 ) ) ;
#5761 = DIRECTION ( 'NONE',  ( 0.000000000000000000, 0.000000000000000000, -1.000000000000000000 ) ) ;
#5762 = ORIENTED_EDGE ( 'NONE', *, *, #1296, .F. ) ;
#5763 = DIRECTION ( 'NONE',  ( 0.000000000000000000, 0.000000000000000000, -1.000000000000000000 ) ) ;
#5764 = EDGE_CURVE ( 'NONE', #5227, #7081, #2742, .T. ) ;
#5765 = VECTOR ( 'NONE', #1572, 1000.000000000000000 ) ;
#5766 = VERTEX_POINT ( 'NONE', #3301 ) ;
#5767 = CARTESIAN_POINT ( 'NONE',  ( 53.33333333333330017, -20.00000000000000000, 165.1500000000000625 ) ) ;
#5768 = DIRECTION ( 'NONE',  ( -1.000000000000000000, 0.000000000000000000, 0.000000000000000000 ) ) ;
#5769 = CONTEXT_DEPENDENT_SHAPE_REPRESENTATION ( #112, #203 ) ;
#5770 = LINE ( 'NONE', #90, #3856 ) ;
#5771 = CARTESIAN_POINT ( 'NONE',  ( 0.000000000000000000, 0.000000000000000000, -140.0000000000000000 ) ) ;
#5772 = SURFACE_STYLE_USAGE ( .BOTH. , #4966 ) ;
#5773 = AXIS2_PLACEMENT_3D ( 'NONE', #3821, #4349, #3202 ) ;
#5774 = ORIENTED_EDGE ( 'NONE', *, *, #2359, .F. ) ;
#5775 = CARTESIAN_POINT ( 'NONE',  ( 4.207491450040567571, -2.029819825146485179, -3.671670828759567407 ) ) ;
#5776 = EDGE_CURVE ( 'NONE', #4178, #7027, #6729, .T. ) ;
#5777 = VERTEX_POINT ( 'NONE', #446 ) ;
#5778 = DIRECTION ( 'NONE',  ( 0.000000000000000000, -1.000000000000000000, 0.000000000000000000 ) ) ;
#5779 = FACE_OUTER_BOUND ( 'NONE', #4378, .T. ) ;
#5780 = CARTESIAN_POINT ( 'NONE',  ( 4.154306624731035846, -2.398490048085128556, -3.721999068284417955 ) ) ;
#5781 = DIRECTION ( 'NONE',  ( 0.000000000000000000, 0.000000000000000000, -1.000000000000000000 ) ) ;
#5782 = COLOUR_RGB ( '',0.8941176470588234615, 0.8941176470588234615, 0.8941176470588234615 ) ;
#5783 = DIRECTION ( 'NONE',  ( 0.000000000000000000, -1.000000000000000000, 0.000000000000000000 ) ) ;
#5784 = VERTEX_POINT ( 'NONE', #5475 ) ;
#5785 = AXIS2_PLACEMENT_3D ( 'NONE', #6323, #2883, #1635 ) ;
#5786 = EDGE_LOOP ( 'NONE', ( #6156, #5814, #3080, #1268 ) ) ;
#5787 = CIRCLE ( 'NONE', #6753, 5.384454397937118664 ) ;
#5788 = CIRCLE ( 'NONE', #2536, 2.041999999999999815 ) ;
#5789 = CARTESIAN_POINT ( 'NONE',  ( 360.0000000000000000, 0.000000000000000000, -123.0000000000000000 ) ) ;
#5790 = DIRECTION ( 'NONE',  ( 0.000000000000000000, -1.000000000000000000, 0.000000000000000000 ) ) ;
#5791 = ORIENTED_EDGE ( 'NONE', *, *, #5596, .T. ) ;
#5792 = SURFACE_SIDE_STYLE ('',( #3454 ) ) ;
#5793 = APPLICATION_CONTEXT ( 'automotive_design' ) ;
#5794 = CARTESIAN_POINT ( 'NONE',  ( 315.0000000000000568, 8.660254037844390851, 140.0000000000000000 ) ) ;
#5795 = ORIENTED_EDGE ( 'NONE', *, *, #3018, .T. ) ;
#5796 = CIRCLE ( 'NONE', #5563, 10.00000000000000000 ) ;
#5797 =( GEOMETRIC_REPRESENTATION_CONTEXT ( 3 ) GLOBAL_UNCERTAINTY_ASSIGNED_CONTEXT ( ( #5943 ) ) GLOBAL_UNIT_ASSIGNED_CONTEXT ( ( #3917, #483, #2348 ) ) REPRESENTATION_CONTEXT ( 'NONE', 'WORKASPACE' ) );
#5798 = SURFACE_STYLE_USAGE ( .BOTH. , #1195 ) ;
#5799 = EDGE_CURVE ( 'NONE', #2185, #4994, #6094, .T. ) ;
#5800 = DIRECTION ( 'NONE',  ( 0.000000000000000000, 0.000000000000000000, 1.000000000000000000 ) ) ;
#5801 = ORIENTED_EDGE ( 'NONE', *, *, #680, .T. ) ;
#5802 = VECTOR ( 'NONE', #3071, 1000.000000000000000 ) ;
#5803 = FACE_OUTER_BOUND ( 'NONE', #2983, .T. ) ;
#5804 = ORIENTED_EDGE ( 'NONE', *, *, #1693, .F. ) ;
#5805 = CARTESIAN_POINT ( 'NONE',  ( 136.6666666666666288, -20.00000000000000000, 162.5000000000000853 ) ) ;
#5806 = DIRECTION ( 'NONE',  ( -0.000000000000000000, 1.000000000000000000, -0.000000000000000000 ) ) ;
#5807 = AXIS2_PLACEMENT_3D ( 'NONE', #5643, #6138, #6702 ) ;
#5808 = CONTEXT_DEPENDENT_SHAPE_REPRESENTATION ( #1769, #4558 ) ;
#5809 = CARTESIAN_POINT ( 'NONE',  ( -0.1404048886732797152, -4.699864953788083888, -3.686887068327043160 ) ) ;
#5810 = CYLINDRICAL_SURFACE ( 'NONE', #6995, 2.649999999999985700 ) ;
#5811 = AXIS2_PLACEMENT_3D ( 'NONE', #5597, #4401, #3914 ) ;
#5812 = FILL_AREA_STYLE ('',( #3257 ) ) ;
#5813 = EDGE_CURVE ( 'NONE', #1784, #1652, #4069, .T. ) ;
#5814 = ORIENTED_EDGE ( 'NONE', *, *, #3432, .T. ) ;
#5815 = CARTESIAN_POINT ( 'NONE',  ( 0.000000000000000000, 2.357898499370433054, -1.951563910473907981E-15 ) ) ;
#5816 = VERTEX_POINT ( 'NONE', #4881 ) ;
#5817 = FACE_OUTER_BOUND ( 'NONE', #4788, .T. ) ;
#5818 = DIRECTION ( 'NONE',  ( 1.000000000000000000, 0.000000000000000000, 0.000000000000000000 ) ) ;
#5819 = CARTESIAN_POINT ( 'NONE',  ( 0.000000000000000000, 0.000000000000000000, 140.0000000000000000 ) ) ;
#5820 = DIRECTION ( 'NONE',  ( 0.000000000000000000, 0.000000000000000000, 1.000000000000000000 ) ) ;
#5821 = ADVANCED_FACE ( 'NONE', ( #326 ), #5994, .F. ) ;
#5822 = VECTOR ( 'NONE', #708, 1000.000000000000000 ) ;
#5823 = DIRECTION ( 'NONE',  ( 0.000000000000000000, -1.000000000000000000, 0.000000000000000000 ) ) ;
#5824 = ORIENTED_EDGE ( 'NONE', *, *, #150, .T. ) ;
#5825 = EDGE_CURVE ( 'NONE', #3722, #2157, #1684, .T. ) ;
#5826 = VERTEX_POINT ( 'NONE', #1554 ) ;
#5827 = CARTESIAN_POINT ( 'NONE',  ( 235.0000000000000000, 8.660254037844390851, 145.0000000000000284 ) ) ;
#5828 = VERTEX_POINT ( 'NONE', #6609 ) ;
#5829 = DIRECTION ( 'NONE',  ( 1.000000000000000000, 0.000000000000000000, 0.000000000000000000 ) ) ;
#5830 = MECHANICAL_DESIGN_GEOMETRIC_PRESENTATION_REPRESENTATION (  '', ( #4522 ), #334 ) ;
#5831 = MANIFOLD_SOLID_BREP ( 'EndChamfer', #4947 ) ;
#5832 = CARTESIAN_POINT ( 'NONE',  ( -4.197477534772231955, 0.8522413273724368521, -3.505042416683225692 ) ) ;
#5833 = EDGE_LOOP ( 'NONE', ( #1047, #1062, #653, #4773 ) ) ;
#5834 = EDGE_CURVE ( 'NONE', #3333, #2910, #6880, .T. ) ;
#5835 = CARTESIAN_POINT ( 'NONE',  ( -0.2277608394786177770, 1.564486285910743648E-15, -12.77499999999999858 ) ) ;
#5836 = LINE ( 'NONE', #4706, #3145 ) ;
#5837 = CARTESIAN_POINT ( 'NONE',  ( 4.197393957002303999, 7.772902908466098641E-14, -3.503767560748929810 ) ) ;
#5838 = CARTESIAN_POINT ( 'NONE',  ( 2.100000000000000089, 0.000000000000000000, -0.2800830152838844622 ) ) ;
#5839 = EDGE_LOOP ( 'NONE', ( #6166, #1634, #1194, #3424 ) ) ;
#5840 = CARTESIAN_POINT ( 'NONE',  ( 470.0000000000000000, -20.00000000000000000, 180.0000000000000284 ) ) ;
#5841 = DIRECTION ( 'NONE',  ( 1.000000000000000000, 0.000000000000000000, 0.000000000000000000 ) ) ;
#5842 = DIRECTION ( 'NONE',  ( 0.000000000000000000, 0.000000000000000000, -1.000000000000000000 ) ) ;
#5843 = LINE ( 'NONE', #91, #7110 ) ;
#5844 =( REPRESENTATION_RELATIONSHIP ('NONE','NONE', #5587, #5294 ) REPRESENTATION_RELATIONSHIP_WITH_TRANSFORMATION ( #5502 )SHAPE_REPRESENTATION_RELATIONSHIP( ) );
#5845 = VERTEX_POINT ( 'NONE', #2707 ) ;
#5846 = DIRECTION ( 'NONE',  ( -0.000000000000000000, 1.000000000000000000, -0.000000000000000000 ) ) ;
#5847 = EDGE_CURVE ( 'NONE', #6041, #2468, #4052, .T. ) ;
#5848 = ORIENTED_EDGE ( 'NONE', *, *, #2791, .F. ) ;
#5849 = EDGE_LOOP ( 'NONE', ( #696, #5114, #5174, #6776 ) ) ;
#5850 = FACE_OUTER_BOUND ( 'NONE', #6921, .T. ) ;
#5851 = LINE ( 'NONE', #1146, #1850 ) ;
#5852 = DIRECTION ( 'NONE',  ( 0.000000000000000000, 0.000000000000000000, -1.000000000000000000 ) ) ;
#5853 = DIRECTION ( 'NONE',  ( 0.000000000000000000, -1.000000000000000000, 1.471414886128461471E-15 ) ) ;
#5854 = DIRECTION ( 'NONE',  ( -0.000000000000000000, 0.000000000000000000, -1.000000000000000000 ) ) ;
#5855 = VERTEX_POINT ( 'NONE', #590 ) ;
#5856 = ORIENTED_EDGE ( 'NONE', *, *, #5825, .T. ) ;
#5857 = EDGE_CURVE ( 'NONE', #3377, #5019, #2427, .T. ) ;
#5858 = CONTEXT_DEPENDENT_SHAPE_REPRESENTATION ( #5258, #3670 ) ;
#5859 = CARTESIAN_POINT ( 'NONE',  ( 405.0000000000000000, -8.660254037844389075, 145.0000000000000284 ) ) ;
#5860 = ORIENTED_EDGE ( 'NONE', *, *, #7172, .T. ) ;
#5861 = DIRECTION ( 'NONE',  ( 1.000000000000000000, 0.000000000000000000, 0.000000000000000000 ) ) ;
#5862 = DIRECTION ( 'NONE',  ( 0.000000000000000000, 0.000000000000000000, 1.000000000000000000 ) ) ;
#5863 = CONICAL_SURFACE ( 'NONE', #2373, 2.041999999999999815, 1.047197551196591858 ) ;
#5864 = VERTEX_POINT ( 'NONE', #1698 ) ;
#5865 = EDGE_CURVE ( 'NONE', #6971, #2488, #5218, .T. ) ;
#5866 = DIRECTION ( 'NONE',  ( -0.000000000000000000, -0.000000000000000000, 1.000000000000000000 ) ) ;
#5867 = VECTOR ( 'NONE', #6839, 1000.000000000000000 ) ;
#5868 = AXIS2_PLACEMENT_3D ( 'NONE', #4965, #1474, #4319 ) ;
#5869 = PLANE ( 'NONE',  #4344 ) ;
#5870 = PRODUCT_DEFINITION_SHAPE ( 'NONE', 'NONE',  #7380 ) ;
#5871 = EDGE_LOOP ( 'NONE', ( #1254, #6664, #1071, #6151 ) ) ;
#5872 = VECTOR ( 'NONE', #1072, 1000.000000000000000 ) ;
#5873 = CARTESIAN_POINT ( 'NONE',  ( 235.0000000000000000, 8.660254037844390851, 139.9990000000000236 ) ) ;
#5874 = ITEM_DEFINED_TRANSFORMATION ( 'NONE', 'NONE', #4954,  #1963 ) ;
#5875 = CARTESIAN_POINT ( 'NONE',  ( 136.6666666666666288, -15.00000000000000000, 159.8500000000001080 ) ) ;
#5876 = DIRECTION ( 'NONE',  ( -1.000000000000000000, -0.000000000000000000, -0.000000000000000000 ) ) ;
#5877 = B_SPLINE_CURVE_WITH_KNOTS ( 'NONE', 3,
 ( #2031, #930, #1529, #1565, #2717, #2680 ),
 .UNSPECIFIED., .F., .F.,
 ( 4, 2, 4 ),
 ( -3.640115492410698714E-06, 0.0002066546034006521879, 0.0004169493222937151081 ),
 .UNSPECIFIED. ) ;
#5878 = PRESENTATION_STYLE_ASSIGNMENT (( #2937 ) ) ;
#5879 = EDGE_LOOP ( 'NONE', ( #1483, #612, #6588, #4421 ) ) ;
#5880 = DIRECTION ( 'NONE',  ( 0.000000000000000000, 0.000000000000000000, -1.000000000000000000 ) ) ;
#5881 = AXIS2_PLACEMENT_3D ( 'NONE', #2346, #6800, #18 ) ;
#5882 = ORIENTED_EDGE ( 'NONE', *, *, #809, .T. ) ;
#5883 = ORIENTED_EDGE ( 'NONE', *, *, #1808, .F. ) ;
#5884 =( REPRESENTATION_RELATIONSHIP ('NONE','NONE', #5587, #951 ) REPRESENTATION_RELATIONSHIP_WITH_TRANSFORMATION ( #3539 )SHAPE_REPRESENTATION_RELATIONSHIP( ) );
#5885 = CARTESIAN_POINT ( 'NONE',  ( 0.000000000000000000, 0.000000000000000000, 0.000000000000000000 ) ) ;
#5886 = CARTESIAN_POINT ( 'NONE',  ( 0.1756481739660539498, -4.720212674038995360, -3.469390959564070620 ) ) ;
#5887 = CARTESIAN_POINT ( 'NONE',  ( 365.0000000000000000, -8.660254037844389075, 145.0000000000000284 ) ) ;
#5888 = CARTESIAN_POINT ( 'NONE',  ( -20.63749999999999574, 0.000000000000000000, 0.000000000000000000 ) ) ;
#5889 = VECTOR ( 'NONE', #2051, 1000.000000000000000 ) ;
#5890 = ADVANCED_FACE ( 'NONE', ( #5633 ), #1076, .F. ) ;
#5891 = CARTESIAN_POINT ( 'NONE',  ( 2.500000000000000000, 2.357898499370433054, -1.951563910473907981E-15 ) ) ;
#5892 = DIRECTION ( 'NONE',  ( -1.000000000000000000, 0.000000000000000000, 0.000000000000000000 ) ) ;
#5893 = ORIENTED_EDGE ( 'NONE', *, *, #2057, .F. ) ;
#5894 = ORIENTED_EDGE ( 'NONE', *, *, #4209, .F. ) ;
#5895 = ITEM_DEFINED_TRANSFORMATION ( 'NONE', 'NONE', #6643,  #1963 ) ;
#5896 = VECTOR ( 'NONE', #6131, 1000.000000000000227 ) ;
#5897 = PLANE ( 'NONE',  #1971 ) ;
#5898 = VERTEX_POINT ( 'NONE', #2878 ) ;
#5899 = PRESENTATION_STYLE_ASSIGNMENT (( #4660 ) ) ;
#5900 = EDGE_CURVE ( 'NONE', #5307, #3104, #6990, .T. ) ;
#5901 = CIRCLE ( 'NONE', #2998, 2.649999999999985700 ) ;
#5902 = AXIS2_PLACEMENT_3D ( 'NONE', #3308, #1597, #365 ) ;
#5903 = DIRECTION ( 'NONE',  ( 0.000000000000000000, 0.000000000000000000, -1.000000000000000000 ) ) ;
#5904 = AXIS2_PLACEMENT_3D ( 'NONE', #4890, #5573, #456 ) ;
#5905 = VECTOR ( 'NONE', #911, 1000.000000000000000 ) ;
#5906 = EDGE_CURVE ( 'NONE', #2399, #153, #5181, .T. ) ;
#5907 = ORIENTED_EDGE ( 'NONE', *, *, #4565, .T. ) ;
#5908 = ORIENTED_EDGE ( 'NONE', *, *, #556, .F. ) ;
#5909 = ORIENTED_EDGE ( 'NONE', *, *, #3778, .F. ) ;
#5910 = DIRECTION ( 'NONE',  ( 1.000000000000000000, 0.000000000000000000, 0.000000000000000000 ) ) ;
#5911 = AXIS2_PLACEMENT_3D ( 'NONE', #3321, #3434, #1059 ) ;
#5912 = CONICAL_SURFACE ( 'NONE', #4708, 2.059999999999998721, 0.9599310885968738161 ) ;
#5913 = EDGE_CURVE ( 'NONE', #2803, #4203, #29, .T. ) ;
#5914 = VERTEX_POINT ( 'NONE', #3952 ) ;
#5915 = VECTOR ( 'NONE', #2611, 1000.000000000000000 ) ;
#5916 = ORIENTED_EDGE ( 'NONE', *, *, #7136, .T. ) ;
#5917 = STYLED_ITEM ( 'NONE', ( #4183 ), #7090 ) ;
#5918 = ADVANCED_FACE ( 'NONE', ( #2777, #2356, #5675, #4653, #6348, #3916, #1666, #6941, #5717, #5119, #1214, #515, #2286 ), #109, .F. ) ;
#5919 = CARTESIAN_POINT ( 'NONE',  ( 285.0000000000000568, 8.660254037844390851, 145.0000000000000284 ) ) ;
#5920 = DIRECTION ( 'NONE',  ( 0.000000000000000000, 0.000000000000000000, 1.000000000000000000 ) ) ;
#5921 = VECTOR ( 'NONE', #3979, 1000.000000000000000 ) ;
#5922 = CARTESIAN_POINT ( 'NONE',  ( 0.000000000000000000, 0.000000000000000000, 0.000000000000000000 ) ) ;
#5923 = VECTOR ( 'NONE', #5226, 1000.000000000000000 ) ;
#5924 = EDGE_LOOP ( 'NONE', ( #6389, #1540 ) ) ;
#5925 = CARTESIAN_POINT ( 'NONE',  ( -19.00000000000000000, 0.000000000000000000, -125.0000000000000000 ) ) ;
#5926 = ORIENTED_EDGE ( 'NONE', *, *, #6493, .F. ) ;
#5927 = CIRCLE ( 'NONE', #4491, 2.649999999999985700 ) ;
#5928 = ORIENTED_EDGE ( 'NONE', *, *, #6072, .F. ) ;
#5929 = CARTESIAN_POINT ( 'NONE',  ( 3.999999999999999112, -1.539600717839012978, -3.300726591567080703 ) ) ;
#5930 = DIRECTION ( 'NONE',  ( 0.000000000000000000, 0.000000000000000000, -1.000000000000000000 ) ) ;
#5931 = CARTESIAN_POINT ( 'NONE',  ( 0.000000000000000000, 0.000000000000000000, -121.0000000000000000 ) ) ;
#5932 = CARTESIAN_POINT ( 'NONE',  ( -4.000000000000000000, -2.309401076758515803, -0.4999999999999995559 ) ) ;
#5933 = EDGE_CURVE ( 'NONE', #1904, #2749, #1946, .T. ) ;
#5934 = DIRECTION ( 'NONE',  ( -0.000000000000000000, -0.000000000000000000, 1.000000000000000000 ) ) ;
#5935 = DIRECTION ( 'NONE',  ( 0.000000000000000000, 0.000000000000000000, 1.000000000000000000 ) ) ;
#5936 = VECTOR ( 'NONE', #1134, 1000.000000000000000 ) ;
#5937 = EDGE_LOOP ( 'NONE', ( #201, #1844, #4780, #4631, #6957, #5152 ) ) ;
#5938 = CARTESIAN_POINT ( 'NONE',  ( 1.391697335622810172, 4.043246145443375461, -3.503898532754365913 ) ) ;
#5939 = ORIENTED_EDGE ( 'NONE', *, *, #7145, .T. ) ;
#5940 = EDGE_CURVE ( 'NONE', #5999, #3484, #1148, .T. ) ;
#5941 = PRODUCT_DEFINITION_SHAPE ( 'NONE', 'NONE',  #7401 ) ;
#5942 = DIRECTION ( 'NONE',  ( -1.000000000000000000, 0.000000000000000000, 0.000000000000000000 ) ) ;
#5943 = UNCERTAINTY_MEASURE_WITH_UNIT (LENGTH_MEASURE( 1.000000000000000082E-05 ), #3917, 'distance_accuracy_value', 'NONE');
#5944 = ORIENTED_EDGE ( 'NONE', *, *, #2691, .F. ) ;
#5945 = EDGE_CURVE ( 'NONE', #1422, #7293, #6320, .T. ) ;
#5946 = VERTEX_POINT ( 'NONE', #5285 ) ;
#5947 = EDGE_CURVE ( 'NONE', #1904, #1563, #2894, .T. ) ;
#5948 = LINE ( 'NONE', #1075, #5648 ) ;
#5949 = CARTESIAN_POINT ( 'NONE',  ( -6.473970235329672780E-16, -4.862606272033106691, -3.745885042887442395 ) ) ;
#5950 = VERTEX_POINT ( 'NONE', #5932 ) ;
#5951 = FACE_OUTER_BOUND ( 'NONE', #2544, .T. ) ;
#5952 = ORIENTED_EDGE ( 'NONE', *, *, #941, .T. ) ;
#5953 = EDGE_CURVE ( 'NONE', #4011, #1413, #5390, .T. ) ;
#5954 = CARTESIAN_POINT ( 'NONE',  ( 303.3333333333333144, -20.00000000000000000, -165.1500000000000625 ) ) ;
#5955 = CONTEXT_DEPENDENT_SHAPE_REPRESENTATION ( #6665, #4789 ) ;
#5956 = FACE_OUTER_BOUND ( 'NONE', #2342, .T. ) ;
#5957 = CARTESIAN_POINT ( 'NONE',  ( 245.0000000000000000, 8.660254037844390851, 145.0000000000000284 ) ) ;
#5958 = SURFACE_STYLE_FILL_AREA ( #5812 ) ;
#5959 = EDGE_LOOP ( 'NONE', ( #4874, #2139 ) ) ;
#5960 = DIRECTION ( 'NONE',  ( 0.000000000000000000, 0.000000000000000000, 1.000000000000000000 ) ) ;
#5961 = PRODUCT_DEFINITION_SHAPE ( 'NONE', 'NONE',  #7350 ) ;
#5962 = VECTOR ( 'NONE', #3443, 1000.000000000000000 ) ;
#5963 = ORIENTED_EDGE ( 'NONE', *, *, #7098, .T. ) ;
#5964 = ORIENTED_EDGE ( 'NONE', *, *, #500, .F. ) ;
#5965 = EDGE_CURVE ( 'NONE', #5144, #6751, #3587, .T. ) ;
#5966 = CARTESIAN_POINT ( 'NONE',  ( 470.0000000000000000, -20.00000000000000000, 180.0000000000000284 ) ) ;
#5967 = LINE ( 'NONE', #7157, #564 ) ;
#5968 = CARTESIAN_POINT ( 'NONE',  ( 365.0000000000000000, 8.660254037844390851, 140.0000000000000000 ) ) ;
#5969 = LINE ( 'NONE', #3550, #5551 ) ;
#5970 = DIRECTION ( 'NONE',  ( -0.000000000000000000, 1.000000000000000000, 0.000000000000000000 ) ) ;
#5971 = CARTESIAN_POINT ( 'NONE',  ( -5.000000000000000888, 8.660254037844390851, 145.0000000000000284 ) ) ;
#5972 = EDGE_LOOP ( 'NONE', ( #1841, #4822, #3028, #14 ) ) ;
#5973 = CARTESIAN_POINT ( 'NONE',  ( 0.000000000000000000, 0.000000000000000000, 125.0000000000000000 ) ) ;
#5974 = EDGE_LOOP ( 'NONE', ( #1090, #280 ) ) ;
#5975 = FACE_OUTER_BOUND ( 'NONE', #2518, .T. ) ;
#5976 = SURFACE_STYLE_FILL_AREA ( #5477 ) ;
#5977 = DIRECTION ( 'NONE',  ( 0.000000000000000000, 1.000000000000000000, 0.000000000000000000 ) ) ;
#5978 = ORIENTED_EDGE ( 'NONE', *, *, #1284, .F. ) ;
#5979 = ORIENTED_EDGE ( 'NONE', *, *, #4260, .F. ) ;
#5980 = LINE ( 'NONE', #3300, #3093 ) ;
#5981 = CARTESIAN_POINT ( 'NONE',  ( 219.9999999999999716, -15.00000000000000000, 165.1500000000000625 ) ) ;
#5982 = EDGE_CURVE ( 'NONE', #450, #541, #2075, .T. ) ;
#5983 = CARTESIAN_POINT ( 'NONE',  ( -0.6666666666666651864, 4.233901974057260098, -3.300726591567081147 ) ) ;
#5984 = DIRECTION ( 'NONE',  ( 0.000000000000000000, -1.000000000000000000, 0.000000000000000000 ) ) ;
#5985 =( REPRESENTATION_RELATIONSHIP ('NONE','NONE', #5587, #5294 ) REPRESENTATION_RELATIONSHIP_WITH_TRANSFORMATION ( #881 )SHAPE_REPRESENTATION_RELATIONSHIP( ) );
#5986 = ORIENTED_EDGE ( 'NONE', *, *, #1240, .F. ) ;
#5987 = AXIS2_PLACEMENT_3D ( 'NONE', #4652, #1794, #2846 ) ;
#5988 = CARTESIAN_POINT ( 'NONE',  ( 4.000000000000000000, -2.511475576507276042, -3.469253905236643565 ) ) ;
#5989 = CONTEXT_DEPENDENT_SHAPE_REPRESENTATION ( #3441, #3413 ) ;
#5990 = CARTESIAN_POINT ( 'NONE',  ( 124.9999999999999858, -8.660254037844389075, 145.0000000000000284 ) ) ;
#5991 = FACE_BOUND ( 'NONE', #2843, .T. ) ;
#5992 = CARTESIAN_POINT ( 'NONE',  ( 120.0000000000000000, 0.000000000000000000, -123.0000000000000000 ) ) ;
#5993 = ORIENTED_EDGE ( 'NONE', *, *, #2918, .T. ) ;
#5994 = CONICAL_SURFACE ( 'NONE', #3580, 2.041999999999999815, 1.047197551196591858 ) ;
#5995 = CARTESIAN_POINT ( 'NONE',  ( -2.805705207896067144, 3.226868319750155312, -3.503898532754364581 ) ) ;
#5996 = AXIS2_PLACEMENT_3D ( 'NONE', #690, #2942, #5245 ) ;
#5997 = EDGE_CURVE ( 'NONE', #4387, #5845, #4234, .T. ) ;
#5998 = ORIENTED_EDGE ( 'NONE', *, *, #2991, .T. ) ;
#5999 = VERTEX_POINT ( 'NONE', #802 ) ;
#6000 = DIRECTION ( 'NONE',  ( 0.000000000000000000, 0.000000000000000000, 1.000000000000000000 ) ) ;
#6001 = CARTESIAN_POINT ( 'NONE',  ( 303.3333333333333144, -25.00000000000000000, -165.1500000000000625 ) ) ;
#6002 = CARTESIAN_POINT ( 'NONE',  ( 195.0000000000000000, -8.660254037844389075, 139.9990000000000236 ) ) ;
#6003 = LINE ( 'NONE', #3822, #1727 ) ;
#6004 = CARTESIAN_POINT ( 'NONE',  ( 2.500000000000000000, -1.178949249685218303, -2.041999999999998039 ) ) ;
#6005 = CARTESIAN_POINT ( 'NONE',  ( 303.3333333333333144, -25.00000000000000000, 162.5000000000000853 ) ) ;
#6006 = EDGE_CURVE ( 'NONE', #807, #5543, #5678, .T. ) ;
#6007 = ORIENTED_EDGE ( 'NONE', *, *, #175, .T. ) ;
#6008 = AXIS2_PLACEMENT_3D ( 'NONE', #4150, #713, #6444 ) ;
#6009 = DIRECTION ( 'NONE',  ( 0.000000000000000000, 0.000000000000000000, -1.000000000000000000 ) ) ;
#6010 = ADVANCED_FACE ( 'NONE', ( #4162 ), #3666, .F. ) ;
#6011 = FACE_OUTER_BOUND ( 'NONE', #6393, .T. ) ;
#6012 = ORIENTED_EDGE ( 'NONE', *, *, #2497, .T. ) ;
#6013 = AXIS2_PLACEMENT_3D ( 'NONE', #7033, #4494, #6787 ) ;
#6014 = SURFACE_SIDE_STYLE ('',( #4284 ) ) ;
#6015 = DIRECTION ( 'NONE',  ( 0.000000000000000000, 0.000000000000000000, 1.000000000000000000 ) ) ;
#6016 = CARTESIAN_POINT ( 'NONE',  ( -31.74999999999995737, 3.061616997868384127E-16, -2.500000000000000888 ) ) ;
#6017 = CIRCLE ( 'NONE', #1930, 2.041999999999999815 ) ;
#6018 = ORIENTED_EDGE ( 'NONE', *, *, #5945, .F. ) ;
#6019 = CARTESIAN_POINT ( 'NONE',  ( 280.0000000000000000, 0.000000000000000000, 123.0000000000000000 ) ) ;
#6020 = ORIENTED_EDGE ( 'NONE', *, *, #6493, .T. ) ;
#6021 = PRODUCT_DEFINITION_SHAPE ( 'NONE', 'NONE',  #7349 ) ;
#6022 = CARTESIAN_POINT ( 'NONE',  ( 405.0000000000000000, 8.660254037844390851, 140.0000000000000000 ) ) ;
#6023 = VECTOR ( 'NONE', #4164, 1000.000000000000000 ) ;
#6024 = AXIS2_PLACEMENT_3D ( 'NONE', #6076, #1019, #5580 ) ;
#6025 = SHAPE_REPRESENTATION ( 'roller', ( #1963 ), #3131 ) ;
#6026 = FACE_OUTER_BOUND ( 'NONE', #5616, .T. ) ;
#6027 = CARTESIAN_POINT ( 'NONE',  ( -19.00000000000000000, 0.000000000000000000, 125.0000000000000000 ) ) ;
#6028 = ORIENTED_EDGE ( 'NONE', *, *, #1527, .T. ) ;
#6029 = AXIS2_PLACEMENT_3D ( 'NONE', #6517, #4379, #2037 ) ;
#6030 = AXIS2_PLACEMENT_3D ( 'NONE', #3882, #5605, #4484 ) ;
#6031 = EDGE_CURVE ( 'NONE', #4072, #5639, #5045, .T. ) ;
#6032 = CARTESIAN_POINT ( 'NONE',  ( 4.000000000000000000, -2.471525695159793035, -3.686886880705770864 ) ) ;
#6033 = ITEM_DEFINED_TRANSFORMATION ( 'NONE', 'NONE', #173,  #1963 ) ;
#6034 = DIRECTION ( 'NONE',  ( -1.000000000000000000, 0.000000000000000000, -0.000000000000000000 ) ) ;
#6035 = CARTESIAN_POINT ( 'NONE',  ( 136.6666666666666288, -20.00000000000000000, -165.1500000000000625 ) ) ;
#6036 = DIRECTION ( 'NONE',  ( 6.123233995736766036E-17, -1.000000000000000000, 0.000000000000000000 ) ) ;
#6037 = VERTEX_POINT ( 'NONE', #3056 ) ;
#6038 = VECTOR ( 'NONE', #2496, 1000.000000000000000 ) ;
#6039 = FACE_OUTER_BOUND ( 'NONE', #3411, .T. ) ;
#6040 =( GEOMETRIC_REPRESENTATION_CONTEXT ( 3 ) GLOBAL_UNCERTAINTY_ASSIGNED_CONTEXT ( ( #1366 ) ) GLOBAL_UNIT_ASSIGNED_CONTEXT ( ( #2021, #3065, #287 ) ) REPRESENTATION_CONTEXT ( 'NONE', 'WORKASPACE' ) );
#6041 = VERTEX_POINT ( 'NONE', #6382 ) ;
#6042 = EDGE_CURVE ( 'NONE', #1419, #5197, #2305, .T. ) ;
#6043 = ORIENTED_EDGE ( 'NONE', *, *, #849, .F. ) ;
#6044 = CARTESIAN_POINT ( 'NONE',  ( 219.9999999999999716, -20.00000000000000000, -165.1500000000000625 ) ) ;
#6045 = DIRECTION ( 'NONE',  ( 0.000000000000000000, 1.000000000000000000, 0.000000000000000000 ) ) ;
#6046 = AXIS2_PLACEMENT_3D ( 'NONE', #3773, #2087, #4939 ) ;
#6047 = AXIS2_PLACEMENT_3D ( 'NONE', #5697, #6222, #2198 ) ;
#6048 = DIRECTION ( 'NONE',  ( 1.000000000000000000, 0.000000000000000000, 0.000000000000000000 ) ) ;
#6049 = CARTESIAN_POINT ( 'NONE',  ( 75.00000000000001421, 8.660254037844390851, 140.0000000000000000 ) ) ;
#6050 = ADVANCED_FACE ( 'NONE', ( #1312 ), #7086, .F. ) ;
#6051 = DIRECTION ( 'NONE',  ( 0.000000000000000000, 0.000000000000000000, 1.000000000000000000 ) ) ;
#6052 = PLANE ( 'NONE',  #6623 ) ;
#6053 = DIRECTION ( 'NONE',  ( -1.000000000000000000, -0.000000000000000000, -0.000000000000000000 ) ) ;
#6054 = AXIS2_PLACEMENT_3D ( 'NONE', #6332, #5265, #115 ) ;
#6055 = ORIENTED_EDGE ( 'NONE', *, *, #3329, .F. ) ;
#6056 = CIRCLE ( 'NONE', #4372, 2.649999999999985700 ) ;
#6057 = DIRECTION ( 'NONE',  ( -0.000000000000000000, -0.000000000000000000, -1.000000000000000000 ) ) ;
#6058 = CARTESIAN_POINT ( 'NONE',  ( -31.74999999999995737, 0.000000000000000000, 2.500000000000000888 ) ) ;
#6059 = EDGE_LOOP ( 'NONE', ( #1456, #1177, #6236, #1999 ) ) ;
#6060 = EDGE_CURVE ( 'NONE', #1207, #7046, #275, .T. ) ;
#6061 = CARTESIAN_POINT ( 'NONE',  ( 114.9999999999999858, 8.660254037844390851, 145.0000000000000284 ) ) ;
#6062 = EDGE_CURVE ( 'NONE', #3602, #6365, #5190, .T. ) ;
#6063 = DIRECTION ( 'NONE',  ( -0.000000000000000000, 0.000000000000000000, -1.000000000000000000 ) ) ;
#6064 = VERTEX_POINT ( 'NONE', #1869 ) ;
#6066 = CONICAL_SURFACE ( 'NONE', #2695, 2.500000000000000888, 0.9599310885968785900 ) ;
#6065 = CARTESIAN_POINT ( 'NONE',  ( 303.3333333333333144, -30.00000000000000355, -162.5000000000000853 ) ) ;
#6067 = ORIENTED_EDGE ( 'NONE', *, *, #5201, .T. ) ;
#6068 = EDGE_CURVE ( 'NONE', #3899, #5639, #5969, .T. ) ;
#6069 = CARTESIAN_POINT ( 'NONE',  ( 235.0000000000000000, -8.660254037844389075, 140.0000000000000000 ) ) ;
#6070 = DIRECTION ( 'NONE',  ( 1.000000000000000000, 0.000000000000000000, 0.000000000000000000 ) ) ;
#6071 = ORIENTED_EDGE ( 'NONE', *, *, #6851, .F. ) ;
#6072 = EDGE_CURVE ( 'NONE', #3535, #2468, #7051, .T. ) ;
#6073 = CARTESIAN_POINT ( 'NONE',  ( 4.197478902586992966, -0.8524102783748346290, -3.505063281295504041 ) ) ;
#6074 = DIRECTION ( 'NONE',  ( 0.000000000000000000, 1.000000000000000000, 0.000000000000000000 ) ) ;
#6075 = DIRECTION ( 'NONE',  ( -1.000000000000000000, 0.000000000000000000, 0.000000000000000000 ) ) ;
#6076 = CARTESIAN_POINT ( 'NONE',  ( 0.000000000000000000, 0.000000000000000000, 123.0000000000000000 ) ) ;
#6077 = ORIENTED_EDGE ( 'NONE', *, *, #1197, .T. ) ;
#6078 = DIRECTION ( 'NONE',  ( -1.000000000000000000, 0.000000000000000000, -0.000000000000000000 ) ) ;
#6079 = ORIENTED_EDGE ( 'NONE', *, *, #500, .T. ) ;
#6080 = PRODUCT_DEFINITION_CONTEXT ( 'detailed design', #6326, 'design' ) ;
#6081 = ORIENTED_EDGE ( 'NONE', *, *, #2864, .F. ) ;
#6082 = CARTESIAN_POINT ( 'NONE',  ( 75.00000000000001421, -8.660254037844389075, 140.0000000000000000 ) ) ;
#6083 = LINE ( 'NONE', #5030, #4137 ) ;
#6084 = CARTESIAN_POINT ( 'NONE',  ( 3.355112389629172576, -2.681727112203168950, -0.2256878752776777242 ) ) ;
#6085 = PLANE ( 'NONE',  #1244 ) ;
#6086 = DIRECTION ( 'NONE',  ( 0.000000000000000000, 0.000000000000000000, -1.000000000000000000 ) ) ;
#6087 = AXIS2_PLACEMENT_3D ( 'NONE', #7242, #2102, #5034 ) ;
#6088 = DIRECTION ( 'NONE',  ( -0.000000000000000000, 0.000000000000000000, 1.000000000000000000 ) ) ;
#6089 = ADVANCED_FACE ( 'NONE', ( #1247 ), #4832, .F. ) ;
#6090 = EDGE_LOOP ( 'NONE', ( #1217, #6616, #5908, #4224 ) ) ;
#6091 = PRODUCT_DEFINITION_SHAPE ( 'NONE', 'NONE',  #7367 ) ;
#6092 = CARTESIAN_POINT ( 'NONE',  ( 2.344047193898588954, 3.265465875126468021, -5.031375706690542042E-16 ) ) ;
#6093 = CARTESIAN_POINT ( 'NONE',  ( 245.0000000000000000, 8.660254037844390851, 140.0000000000000000 ) ) ;
#6094 = LINE ( 'NONE', #3135, #7315 ) ;
#6095 = B_SPLINE_CURVE_WITH_KNOTS ( 'NONE', 3,
 ( #2466, #1835, #5389, #4793, #6530, #6489 ),
 .UNSPECIFIED., .F., .F.,
 ( 4, 2, 4 ),
 ( 0.000000000000000000, 0.0002095117440854730670, 0.0004190234881709461339 ),
 .UNSPECIFIED. ) ;
#6096 = PLANE ( 'NONE',  #2654 ) ;
#6097 = CARTESIAN_POINT ( 'NONE',  ( 2.500000000000000000, -1.178949249685213863, 2.042000000000002924 ) ) ;
#6098 = EDGE_CURVE ( 'NONE', #2399, #2352, #1137, .T. ) ;
#6099 = ORIENTED_EDGE ( 'NONE', *, *, #3591, .F. ) ;
#6100 = ORIENTED_EDGE ( 'NONE', *, *, #7320, .T. ) ;
#6101 = EDGE_CURVE ( 'NONE', #3638, #5278, #4417, .T. ) ;
#6102 = CARTESIAN_POINT ( 'NONE',  ( 240.0000000000000000, 0.000000000000000000, 0.000000000000000000 ) ) ;
#6103 = ORIENTED_EDGE ( 'NONE', *, *, #5644, .F. ) ;
#6104 = CARTESIAN_POINT ( 'NONE',  ( 315.0000000000000568, 8.660254037844390851, 139.9990000000000236 ) ) ;
#6105 = CARTESIAN_POINT ( 'NONE',  ( 136.6666666666666288, -14.99999999999999822, 162.5000000000000853 ) ) ;
#6106 = FACE_OUTER_BOUND ( 'NONE', #5663, .T. ) ;
#6107 = EDGE_CURVE ( 'NONE', #5434, #5227, #6003, .T. ) ;
#6108 = VERTEX_POINT ( 'NONE', #1031 ) ;
#6109 = LINE ( 'NONE', #5954, #3121 ) ;
#6110 = DIRECTION ( 'NONE',  ( 0.000000000000000000, 0.000000000000000000, -1.000000000000000000 ) ) ;
#6111 = FACE_OUTER_BOUND ( 'NONE', #333, .T. ) ;
#6112 = DIRECTION ( 'NONE',  ( 1.000000000000000000, 0.000000000000000000, 0.000000000000000000 ) ) ;
#6113 = ORIENTED_EDGE ( 'NONE', *, *, #1453, .F. ) ;
#6114 = CARTESIAN_POINT ( 'NONE',  ( -1.393927851585477606, 4.043713361053528743, -3.526374918436835149 ) ) ;
#6115 = AXIS2_PLACEMENT_3D ( 'NONE', #5067, #579, #5586 ) ;
#6116 = EDGE_LOOP ( 'NONE', ( #2442, #40, #1961, #7128 ) ) ;
#6117 = ORIENTED_EDGE ( 'NONE', *, *, #5048, .T. ) ;
#6118 = DIRECTION ( 'NONE',  ( -1.000000000000000000, -0.000000000000000000, -0.000000000000000000 ) ) ;
#6119 = CARTESIAN_POINT ( 'NONE',  ( -4.197393957002303999, -7.773935952363655451E-14, -3.503767560748929810 ) ) ;
#6120 = CARTESIAN_POINT ( 'NONE',  ( 5.384454397937118664, 0.000000000000000000, -4.484454397937119197 ) ) ;
#6121 = CARTESIAN_POINT ( 'NONE',  ( 470.0000000000000000, -20.00000000000000000, -200.0000000000000000 ) ) ;
#6122 = VECTOR ( 'NONE', #6319, 1000.000000000000000 ) ;
#6123 = DIRECTION ( 'NONE',  ( -0.5000000000000019984, -0.8660254037844375974, 0.000000000000000000 ) ) ;
#6124 = LINE ( 'NONE', #5555, #5905 ) ;
#6125 = ORIENTED_EDGE ( 'NONE', *, *, #5094, .F. ) ;
#6126 = DIRECTION ( 'NONE',  ( -1.000000000000000000, -0.000000000000000000, -0.000000000000000000 ) ) ;
#6127 = PLANE ( 'NONE',  #2558 ) ;
#6128 = EDGE_CURVE ( 'NONE', #3198, #5656, #3165, .T. ) ;
#6129 = DIRECTION ( 'NONE',  ( 1.000000000000000000, 0.000000000000000000, 0.000000000000000000 ) ) ;
#6130 = SHAPE_REPRESENTATION_RELATIONSHIP ( 'NONE' , 'NONE' ,  #5294, #5044 ) ;
#6131 = DIRECTION ( 'NONE',  ( 0.9396926207859138680, 1.150791560227856926E-16, -0.3420201433256536139 ) ) ;
#6132 = DIRECTION ( 'NONE',  ( -0.000000000000000000, -0.000000000000000000, 1.000000000000000000 ) ) ;
#6133 = ORIENTED_EDGE ( 'NONE', *, *, #3648, .T. ) ;
#6134 = EDGE_LOOP ( 'NONE', ( #2780, #2461, #4061, #3359 ) ) ;
#6135 = DIRECTION ( 'NONE',  ( 0.000000000000000000, 0.000000000000000000, 1.000000000000000000 ) ) ;
#6136 = EDGE_LOOP ( 'NONE', ( #3323, #2437 ) ) ;
#6137 =( REPRESENTATION_RELATIONSHIP ('NONE','NONE', #5587, #5294 ) REPRESENTATION_RELATIONSHIP_WITH_TRANSFORMATION ( #3861 )SHAPE_REPRESENTATION_RELATIONSHIP( ) );
#6138 = DIRECTION ( 'NONE',  ( -0.000000000000000000, -0.000000000000000000, -1.000000000000000000 ) ) ;
#6139 = EDGE_CURVE ( 'NONE', #2951, #2185, #1582, .T. ) ;
#6140 = VECTOR ( 'NONE', #6048, 1000.000000000000000 ) ;
#6141 = DIRECTION ( 'NONE',  ( 0.000000000000000000, 0.000000000000000000, -1.000000000000000000 ) ) ;
#6142 = DIRECTION ( 'NONE',  ( 0.000000000000000000, 0.000000000000000000, -1.000000000000000000 ) ) ;
#6143 = ORIENTED_EDGE ( 'NONE', *, *, #6547, .T. ) ;
#6144 = CARTESIAN_POINT ( 'NONE',  ( 5.000000000000004441, 0.000000000000000000, 0.000000000000000000 ) ) ;
#6145 = CONTEXT_DEPENDENT_SHAPE_REPRESENTATION ( #6512, #1156 ) ;
#6146 = CARTESIAN_POINT ( 'NONE',  ( -2.000000000000006661, 3.464101615137750834, 0.000000000000000000 ) ) ;
#6147 = CARTESIAN_POINT ( 'NONE',  ( -20.63749999999999574, 0.000000000000000000, 0.000000000000000000 ) ) ;
#6148 = ADVANCED_FACE ( 'NONE', ( #2052 ), #2100, .T. ) ;
#6149 = CLOSED_SHELL ( 'NONE', ( #7330, #4431, #5351, #1600, #2612, #4668, #3793, #4674, #6089, #2242, #2949, #4923, #5572, #7231, #1206, #1275, #3052, #2650, #6646, #2483, #6693, #3962, #4065, #143, #4142, #6187 ) ) ;
#6150 = DIRECTION ( 'NONE',  ( 0.000000000000000000, 0.000000000000000000, 1.000000000000000000 ) ) ;
#6151 = ORIENTED_EDGE ( 'NONE', *, *, #2140, .F. ) ;
#6152 = DIRECTION ( 'NONE',  ( 1.000000000000000000, 0.000000000000000000, 0.000000000000000000 ) ) ;
#6153 = AXIS2_PLACEMENT_3D ( 'NONE', #4369, #6135, #1003 ) ;
#6154 = AXIS2_PLACEMENT_3D ( 'NONE', #4797, #1315, #760 ) ;
#6155 = AXIS2_PLACEMENT_3D ( 'NONE', #1399, #6535, #7204 ) ;
#6156 = ORIENTED_EDGE ( 'NONE', *, *, #1153, .T. ) ;
#6157 = ORIENTED_EDGE ( 'NONE', *, *, #1661, .T. ) ;
#6158 = PLANE ( 'NONE',  #4179 ) ;
#6159 = DIRECTION ( 'NONE',  ( 0.000000000000000000, 0.000000000000000000, -1.000000000000000000 ) ) ;
#6160 = CARTESIAN_POINT ( 'NONE',  ( 386.6666666666666288, -15.00000000000000000, 165.1500000000000625 ) ) ;
#6161 = DIRECTION ( 'NONE',  ( 0.000000000000000000, 0.000000000000000000, -1.000000000000000000 ) ) ;
#6162 = VECTOR ( 'NONE', #2430, 1000.000000000000000 ) ;
#6163 = FACE_OUTER_BOUND ( 'NONE', #2897, .T. ) ;
#6164 = UNCERTAINTY_MEASURE_WITH_UNIT (LENGTH_MEASURE( 1.000000000000000082E-05 ), #1926, 'distance_accuracy_value', 'NONE');
#6165 = DIRECTION ( 'NONE',  ( 0.000000000000000000, 0.000000000000000000, 1.000000000000000000 ) ) ;
#6166 = ORIENTED_EDGE ( 'NONE', *, *, #7172, .F. ) ;
#6167 = AXIS2_PLACEMENT_3D ( 'NONE', #1788, #2902, #5207 ) ;
#6168 = EDGE_CURVE ( 'NONE', #5089, #5019, #909, .T. ) ;
#6169 = DIRECTION ( 'NONE',  ( -0.000000000000000000, -0.000000000000000000, 1.000000000000000000 ) ) ;
#6170 = DIRECTION ( 'NONE',  ( 0.000000000000000000, -1.000000000000000000, 0.000000000000000000 ) ) ;
#6171 = CARTESIAN_POINT ( 'NONE',  ( 35.00000000000000000, 8.660254037844390851, 145.0000000000000284 ) ) ;
#6172 = DIRECTION ( 'NONE',  ( 0.000000000000000000, -0.000000000000000000, -1.000000000000000000 ) ) ;
#6173 = PRODUCT_CONTEXT ( 'NONE', #3877, 'mechanical' ) ;
#6174 = VECTOR ( 'NONE', #2444, 1000.000000000000000 ) ;
#6175 = ORIENTED_EDGE ( 'NONE', *, *, #6789, .F. ) ;
#6176 = VERTEX_POINT ( 'NONE', #6121 ) ;
#6177 = B_SPLINE_CURVE_WITH_KNOTS ( 'NONE', 3,
 ( #3632, #4732, #7088, #134, #3057, #1902 ),
 .UNSPECIFIED., .F., .F.,
 ( 4, 2, 4 ),
 ( 0.002365888236228001588, 0.003551327329835089319, 0.004736766423442177049 ),
 .UNSPECIFIED. ) ;
#6178 = DIRECTION ( 'NONE',  ( 1.000000000000000000, 0.000000000000000000, 0.000000000000000000 ) ) ;
#6179 = VERTEX_POINT ( 'NONE', #317 ) ;
#6180 = CIRCLE ( 'NONE', #5440, 2.041999999999999815 ) ;
#6181 = CARTESIAN_POINT ( 'NONE',  ( 2.500000000000000000, -1.178949249685213863, 2.042000000000002924 ) ) ;
#6182 = DIRECTION ( 'NONE',  ( 0.000000000000000000, -0.000000000000000000, 1.000000000000000000 ) ) ;
#6183 = DIRECTION ( 'NONE',  ( -0.000000000000000000, 1.000000000000000000, 0.000000000000000000 ) ) ;
#6184 = EDGE_CURVE ( 'NONE', #3509, #4048, #4999, .T. ) ;
#6185 = ORIENTED_EDGE ( 'NONE', *, *, #1164, .F. ) ;
#6186 = APPLICATION_CONTEXT ( 'automotive_design' ) ;
#6187 = ADVANCED_FACE ( 'NONE', ( #2012 ), #4870, .F. ) ;
#6188 = FACE_BOUND ( 'NONE', #5924, .T. ) ;
#6189 = DIRECTION ( 'NONE',  ( 0.000000000000000000, 1.000000000000000000, 0.000000000000000000 ) ) ;
#6190 = VECTOR ( 'NONE', #5862, 1000.000000000000000 ) ;
#6191 = DIRECTION ( 'NONE',  ( 0.000000000000000000, 0.000000000000000000, 1.000000000000000000 ) ) ;
#6192 = ORIENTED_EDGE ( 'NONE', *, *, #6882, .T. ) ;
#6193 = CARTESIAN_POINT ( 'NONE',  ( 0.000000000000000000, 0.000000000000000000, 0.000000000000000000 ) ) ;
#6194 = EDGE_CURVE ( 'NONE', #3982, #5845, #5550, .T. ) ;
#6195 = ORIENTED_EDGE ( 'NONE', *, *, #5635, .T. ) ;
#6196 = ORIENTED_EDGE ( 'NONE', *, *, #6883, .T. ) ;
#6197 = DIRECTION ( 'NONE',  ( 1.000000000000000000, 0.000000000000000000, 0.000000000000000000 ) ) ;
#6198 = CARTESIAN_POINT ( 'NONE',  ( 3.472371940585993855, 2.614027278893175321, -3.320322319201766792 ) ) ;
#6199 = CONTEXT_DEPENDENT_SHAPE_REPRESENTATION ( #5091, #6091 ) ;
#6200 = CARTESIAN_POINT ( 'NONE',  ( -20.63749999999999574, 1.653273178848927261E-15, 13.50000000000000355 ) ) ;
#6201 = DIRECTION ( 'NONE',  ( -1.000000000000000000, -0.000000000000000000, -0.000000000000000000 ) ) ;
#6202 = CIRCLE ( 'NONE', #3705, 13.29999999999999893 ) ;
#6203 = DIRECTION ( 'NONE',  ( 0.000000000000000000, 0.000000000000000000, 1.000000000000000000 ) ) ;
#6204 = CARTESIAN_POINT ( 'NONE',  ( 84.99999999999998579, 8.660254037844390851, 140.0000000000000000 ) ) ;
#6205 = EDGE_CURVE ( 'NONE', #153, #4993, #3628, .T. ) ;
#6206 = ORIENTED_EDGE ( 'NONE', *, *, #484, .F. ) ;
#6207 = DIRECTION ( 'NONE',  ( -0.000000000000000000, -0.000000000000000000, -1.000000000000000000 ) ) ;
#6208 = CARTESIAN_POINT ( 'NONE',  ( 53.33333333333330017, -25.00000000000000000, 162.5000000000000853 ) ) ;
#6209 = FACE_OUTER_BOUND ( 'NONE', #1763, .T. ) ;
#6210 = SURFACE_STYLE_FILL_AREA ( #3954 ) ;
#6211 = ORIENTED_EDGE ( 'NONE', *, *, #1318, .F. ) ;
#6212 = EDGE_LOOP ( 'NONE', ( #1261, #570, #791, #2224 ) ) ;
#6213 = APPLICATION_PROTOCOL_DEFINITION ( 'draft international standard', 'automotive_design', 1998, #3717 ) ;
#6214 = ORIENTED_EDGE ( 'NONE', *, *, #660, .T. ) ;
#6215 = LINE ( 'NONE', #2397, #6409 ) ;
#6216 = DIRECTION ( 'NONE',  ( 0.000000000000000000, 0.000000000000000000, 1.000000000000000000 ) ) ;
#6217 = ORIENTED_EDGE ( 'NONE', *, *, #5359, .F. ) ;
#6218 = FACE_OUTER_BOUND ( 'NONE', #6869, .T. ) ;
#6219 = FACE_BOUND ( 'NONE', #2081, .T. ) ;
#6220 = EDGE_CURVE ( 'NONE', #3083, #598, #2314, .T. ) ;
#6221 = DIRECTION ( 'NONE',  ( 0.000000000000000000, 0.000000000000000000, 1.000000000000000000 ) ) ;
#6222 = DIRECTION ( 'NONE',  ( 0.000000000000000000, 0.000000000000000000, 1.000000000000000000 ) ) ;
#6223 = ORIENTED_EDGE ( 'NONE', *, *, #7103, .T. ) ;
#6224 = CARTESIAN_POINT ( 'NONE',  ( 53.33333333333330017, -20.00000000000000000, 162.5000000000000853 ) ) ;
#6225 = ORIENTED_EDGE ( 'NONE', *, *, #1995, .T. ) ;
#6226 = ORIENTED_EDGE ( 'NONE', *, *, #1955, .T. ) ;
#6227 = CARTESIAN_POINT ( 'NONE',  ( 0.000000000000000000, 0.000000000000000000, 140.0000000000000000 ) ) ;
#6228 = CARTESIAN_POINT ( 'NONE',  ( 0.6666666666666689611, 4.233901974057261874, -3.300726591567082480 ) ) ;
#6229 = FACE_OUTER_BOUND ( 'NONE', #7163, .T. ) ;
#6230 = EDGE_CURVE ( 'NONE', #3397, #4557, #6645, .T. ) ;
#6231 = ORIENTED_EDGE ( 'NONE', *, *, #3521, .T. ) ;
#6232 = LINE ( 'NONE', #5036, #2071 ) ;
#6233 = VECTOR ( 'NONE', #385, 1000.000000000000000 ) ;
#6234 = EDGE_CURVE ( 'NONE', #2174, #1932, #4601, .T. ) ;
#6235 =( REPRESENTATION_RELATIONSHIP ('NONE','NONE', #5587, #5023 ) REPRESENTATION_RELATIONSHIP_WITH_TRANSFORMATION ( #6964 )SHAPE_REPRESENTATION_RELATIONSHIP( ) );
#6236 = ORIENTED_EDGE ( 'NONE', *, *, #7004, .F. ) ;
#6237 = FACE_BOUND ( 'NONE', #383, .T. ) ;
#6238 = DIRECTION ( 'NONE',  ( 0.000000000000000000, 1.000000000000000000, 0.000000000000000000 ) ) ;
#6239 = CARTESIAN_POINT ( 'NONE',  ( 75.00000000000001421, 8.660254037844390851, 145.0000000000000284 ) ) ;
#6240 = DIRECTION ( 'NONE',  ( -1.000000000000000000, 0.000000000000000000, 0.000000000000000000 ) ) ;
#6241 = EDGE_CURVE ( 'NONE', #3535, #2072, #4273, .T. ) ;
#6242 = SURFACE_SIDE_STYLE ('',( #6210 ) ) ;
#6243 = AXIS2_PLACEMENT_3D ( 'NONE', #1663, #1695, #3334 ) ;
#6244 = ORIENTED_EDGE ( 'NONE', *, *, #7160, .T. ) ;
#6245 = ORIENTED_EDGE ( 'NONE', *, *, #1159, .F. ) ;
#6246 = PRODUCT_CONTEXT ( 'NONE', #7329, 'mechanical' ) ;
#6247 = VERTEX_POINT ( 'NONE', #6566 ) ;
#6248 = CARTESIAN_POINT ( 'NONE',  ( 470.0000000000000000, -20.00000000000000000, -200.0000000000000000 ) ) ;
#6249 = AXIS2_PLACEMENT_3D ( 'NONE', #3230, #7268, #6707 ) ;
#6250 = CARTESIAN_POINT ( 'NONE',  ( 1.393927851585479161, -4.043713361053543842, -3.526374918436840922 ) ) ;
#6251 = ORIENTED_EDGE ( 'NONE', *, *, #768, .T. ) ;
#6252 = DIRECTION ( 'NONE',  ( 0.000000000000000000, 0.000000000000000000, 1.000000000000000000 ) ) ;
#6253 = AXIS2_PLACEMENT_3D ( 'NONE', #316, #5503, #6644 ) ;
#6254 = FACE_BOUND ( 'NONE', #5013, .T. ) ;
#6255 = VECTOR ( 'NONE', #4893, 1000.000000000000000 ) ;
#6256 = DIRECTION ( 'NONE',  ( 1.000000000000000000, 0.000000000000000000, 0.000000000000000000 ) ) ;
#6257 = DIRECTION ( 'NONE',  ( 1.000000000000000000, 0.000000000000000000, 0.000000000000000000 ) ) ;
#6258 = EDGE_LOOP ( 'NONE', ( #4581, #5681, #7131, #5330 ) ) ;
#6259 = CARTESIAN_POINT ( 'NONE',  ( -20.63749999999999574, 1.564486285910743648E-15, 12.77499999999999858 ) ) ;
#6260 = EDGE_CURVE ( 'NONE', #3709, #5460, #4225, .T. ) ;
#6261 = CIRCLE ( 'NONE', #866, 19.00000000000000000 ) ;
#6262 = EDGE_LOOP ( 'NONE', ( #3389, #7261, #2200, #6679 ) ) ;
#6263 = CARTESIAN_POINT ( 'NONE',  ( 136.6666666666666288, -25.00000000000000000, -165.1500000000000625 ) ) ;
#6264 = CARTESIAN_POINT ( 'NONE',  ( 136.6666666666666288, -20.00000000000000000, -165.1500000000000625 ) ) ;
#6265 = ITEM_DEFINED_TRANSFORMATION ( 'NONE', 'NONE', #1815,  #1963 ) ;
#6266 = LINE ( 'NONE', #3363, #5395 ) ;
#6267 = CARTESIAN_POINT ( 'NONE',  ( 124.9999999999999858, 8.660254037844390851, 140.0000000000000000 ) ) ;
#6268 = AXIS2_PLACEMENT_3D ( 'NONE', #833, #278, #3520 ) ;
#6269 = EDGE_LOOP ( 'NONE', ( #111, #5292, #576, #5193 ) ) ;
#6270 = AXIS2_PLACEMENT_3D ( 'NONE', #1089, #6824, #6303 ) ;
#6271 = CARTESIAN_POINT ( 'NONE',  ( 315.0000000000000568, -8.660254037844389075, 140.0000000000000000 ) ) ;
#6272 = CIRCLE ( 'NONE', #5080, 11.00000000000000000 ) ;
#6273 = AXIS2_PLACEMENT_3D ( 'NONE', #3205, #4871, #4912 ) ;
#6274 = ADVANCED_FACE ( 'NONE', ( #3701 ), #6085, .F. ) ;
#6275 = VERTEX_POINT ( 'NONE', #1546 ) ;
#6276 = EDGE_CURVE ( 'NONE', #4634, #5950, #2767, .T. ) ;
#6277 = CARTESIAN_POINT ( 'NONE',  ( 2.000000000000005329, -3.464101615137751722, 0.000000000000000000 ) ) ;
#6278 = CARTESIAN_POINT ( 'NONE',  ( 0.000000000000000000, -1.178949249685218303, -2.041999999999998039 ) ) ;
#6279 = AXIS2_PLACEMENT_3D ( 'NONE', #7211, #2073, #962 ) ;
#6280 = AXIS2_PLACEMENT_3D ( 'NONE', #5136, #2860, #6335 ) ;
#6281 = LINE ( 'NONE', #5716, #6945 ) ;
#6282 = DIRECTION ( 'NONE',  ( 0.000000000000000000, 0.000000000000000000, 1.000000000000000000 ) ) ;
#6283 = TOROIDAL_SURFACE ( 'NONE', #5083, 5.384454397937118664, 0.5155456020628804703 ) ;
#6284 = CARTESIAN_POINT ( 'NONE',  ( 75.00000000000001421, -8.660254037844389075, 139.9990000000000236 ) ) ;
#6285 =( REPRESENTATION_RELATIONSHIP ('NONE','NONE', #5587, #5294 ) REPRESENTATION_RELATIONSHIP_WITH_TRANSFORMATION ( #5377 )SHAPE_REPRESENTATION_RELATIONSHIP( ) );
#6286 = VECTOR ( 'NONE', #2574, 1000.000000000000000 ) ;
#6287 = ORIENTED_EDGE ( 'NONE', *, *, #2824, .T. ) ;
#6288 = ORIENTED_EDGE ( 'NONE', *, *, #1730, .T. ) ;
#6289 = ADVANCED_FACE ( 'NONE', ( #4017 ), #6801, .F. ) ;
#6290 =( LENGTH_UNIT ( ) NAMED_UNIT ( * ) SI_UNIT ( .MILLI., .METRE. ) );
#6291 = ORIENTED_EDGE ( 'NONE', *, *, #6360, .T. ) ;
#6292 = AXIS2_PLACEMENT_3D ( 'NONE', #6834, #6867, #2169 ) ;
#6293 = AXIS2_PLACEMENT_3D ( 'NONE', #4264, #3194, #6036 ) ;
#6294 = DIRECTION ( 'NONE',  ( -0.000000000000000000, -0.000000000000000000, 1.000000000000000000 ) ) ;
#6295 = AXIS2_PLACEMENT_3D ( 'NONE', #2055, #1512, #6165 ) ;
#6296 = DIRECTION ( 'NONE',  ( 0.000000000000000000, 0.000000000000000000, -1.000000000000000000 ) ) ;
#6297 = AXIS2_PLACEMENT_3D ( 'NONE', #1914, #3804, #5407 ) ;
#6298 = ORIENTED_EDGE ( 'NONE', *, *, #4021, .T. ) ;
#6299 = ADVANCED_FACE ( 'NONE', ( #2211 ), #887, .T. ) ;
#6300 = CIRCLE ( 'NONE', #4977, 2.055000000000000160 ) ;
#6301 = FACE_BOUND ( 'NONE', #2841, .T. ) ;
#6302 = CARTESIAN_POINT ( 'NONE',  ( 84.99999999999998579, -8.660254037844389075, 140.0000000000000000 ) ) ;
#6303 = DIRECTION ( 'NONE',  ( 1.000000000000000000, 0.000000000000000000, 0.000000000000000000 ) ) ;
#6304 = AXIS2_PLACEMENT_3D ( 'NONE', #6963, #2934, #6311 ) ;
#6305 = ORIENTED_EDGE ( 'NONE', *, *, #680, .F. ) ;
#6306 = PRODUCT_DEFINITION_SHAPE ( 'NONE', 'NONE',  #7396 ) ;
#6307 = DIRECTION ( 'NONE',  ( 0.000000000000000000, -0.000000000000000000, -1.000000000000000000 ) ) ;
#6308 = EDGE_LOOP ( 'NONE', ( #3064, #5474 ) ) ;
#6309 = DIRECTION ( 'NONE',  ( -0.000000000000000000, -0.000000000000000000, -1.000000000000000000 ) ) ;
#6310 = CIRCLE ( 'NONE', #1636, 2.649999999999985700 ) ;
#6311 = DIRECTION ( 'NONE',  ( -1.000000000000000000, 0.000000000000000000, 0.000000000000000000 ) ) ;
#6312 = CARTESIAN_POINT ( 'NONE',  ( 386.6666666666666288, -20.00000000000000000, -159.8500000000001080 ) ) ;
#6313 = DIRECTION ( 'NONE',  ( 1.000000000000000000, 0.000000000000000000, -0.000000000000000000 ) ) ;
#6314 = ORIENTED_EDGE ( 'NONE', *, *, #3589, .F. ) ;
#6315 = DIRECTION ( 'NONE',  ( 0.000000000000000000, 0.000000000000000000, -1.000000000000000000 ) ) ;
#6316 = ORIENTED_EDGE ( 'NONE', *, *, #2779, .T. ) ;
#6317 = DIRECTION ( 'NONE',  ( 0.000000000000000000, -1.000000000000000000, 0.000000000000000000 ) ) ;
#6318 = DIRECTION ( 'NONE',  ( 1.000000000000000000, 0.000000000000000000, 0.000000000000000000 ) ) ;
#6319 = DIRECTION ( 'NONE',  ( 1.000000000000000000, 0.000000000000000000, 0.000000000000000000 ) ) ;
#6320 = LINE ( 'NONE', #4585, #6162 ) ;
#6321 = EDGE_CURVE ( 'NONE', #2674, #5646, #4615, .T. ) ;
#6322 = VERTEX_POINT ( 'NONE', #5070 ) ;
#6323 = CARTESIAN_POINT ( 'NONE',  ( 440.0000000000000000, 0.000000000000000000, -123.0000000000000000 ) ) ;
#6324 = ORIENTED_EDGE ( 'NONE', *, *, #2889, .F. ) ;
#6325 =( LENGTH_UNIT ( ) NAMED_UNIT ( * ) SI_UNIT ( .MILLI., .METRE. ) );
#6326 = APPLICATION_CONTEXT ( 'automotive_design' ) ;
#6327 = EDGE_CURVE ( 'NONE', #3673, #5144, #6341, .T. ) ;
#6328 = AXIS2_PLACEMENT_3D ( 'NONE', #6706, #571, #4564 ) ;
#6329 = DIRECTION ( 'NONE',  ( -0.000000000000000000, -0.000000000000000000, 1.000000000000000000 ) ) ;
#6330 = EDGE_LOOP ( 'NONE', ( #4647, #2181, #624, #1594, #394 ) ) ;
#6331 = CARTESIAN_POINT ( 'NONE',  ( -3.680118525130244400, 2.494084732383327285, -0.3507732604232449702 ) ) ;
#6332 = CARTESIAN_POINT ( 'NONE',  ( 2.500000000000000000, 2.357898499370433054, -1.951563910473907981E-15 ) ) ;
#6333 = EDGE_CURVE ( 'NONE', #2446, #3965, #185, .T. ) ;
#6334 = VERTEX_POINT ( 'NONE', #6267 ) ;
#6335 = DIRECTION ( 'NONE',  ( 0.000000000000000000, 0.000000000000000000, 1.000000000000000000 ) ) ;
#6336 = EDGE_LOOP ( 'NONE', ( #7275, #4188 ) ) ;
#6337 = DIRECTION ( 'NONE',  ( 0.000000000000000000, 0.000000000000000000, 1.000000000000000000 ) ) ;
#6338 = DIRECTION ( 'NONE',  ( -1.000000000000000000, 0.000000000000000000, 0.000000000000000000 ) ) ;
#6339 = ITEM_DEFINED_TRANSFORMATION ( 'NONE', 'NONE', #2433,  #1963 ) ;
#6340 = CARTESIAN_POINT ( 'NONE',  ( 1.567478505476134606E-15, 4.618802153517012066, -3.433295621305382905 ) ) ;
#6341 = LINE ( 'NONE', #5625, #3138 ) ;
#6342 = VERTEX_POINT ( 'NONE', #1066 ) ;
#6343 = CARTESIAN_POINT ( 'NONE',  ( 53.33333333333330017, -20.00000000000000000, -162.5000000000000853 ) ) ;
#6344 = ORIENTED_EDGE ( 'NONE', *, *, #6948, .F. ) ;
#6345 = CARTESIAN_POINT ( 'NONE',  ( 0.3208286057739604957, -4.433571671609698228, -0.3503314178412692548 ) ) ;
#6346 = CARTESIAN_POINT ( 'NONE',  ( 219.9999999999999716, -20.00000000000000000, 159.8500000000001080 ) ) ;
#6347 = CARTESIAN_POINT ( 'NONE',  ( 114.9999999999999858, -8.660254037844389075, 140.0000000000000000 ) ) ;
#6348 = FACE_BOUND ( 'NONE', #3345, .T. ) ;
#6349 = DIRECTION ( 'NONE',  ( 0.000000000000000000, -0.000000000000000000, -1.000000000000000000 ) ) ;
#6350 = ORIENTED_EDGE ( 'NONE', *, *, #2281, .F. ) ;
#6351 = EDGE_CURVE ( 'NONE', #3238, #1780, #5033, .T. ) ;
#6352 = VERTEX_POINT ( 'NONE', #53 ) ;
#6353 = PRODUCT_DEFINITION_SHAPE ( 'NONE', 'NONE',  #7387 ) ;
#6354 = CARTESIAN_POINT ( 'NONE',  ( 0.000000000000000000, 0.000000000000000000, 0.000000000000000000 ) ) ;
#6355 = AXIS2_PLACEMENT_3D ( 'NONE', #4476, #5007, #2144 ) ;
#6356 = VECTOR ( 'NONE', #1665, 1000.000000000000114 ) ;
#6357 = AXIS2_PLACEMENT_3D ( 'NONE', #1813, #3040, #3498 ) ;
#6358 = LINE ( 'NONE', #1294, #3037 ) ;
#6359 = ORIENTED_EDGE ( 'NONE', *, *, #809, .F. ) ;
#6360 = EDGE_CURVE ( 'NONE', #3466, #5483, #702, .T. ) ;
#6361 = PLANE ( 'NONE',  #2771 ) ;
#6362 = PLANE ( 'NONE',  #6054 ) ;
#6363 = ORIENTED_EDGE ( 'NONE', *, *, #6107, .F. ) ;
#6364 = DIRECTION ( 'NONE',  ( 0.000000000000000000, 0.000000000000000000, 1.000000000000000000 ) ) ;
#6365 = VERTEX_POINT ( 'NONE', #506 ) ;
#6366 = AXIS2_PLACEMENT_3D ( 'NONE', #2561, #423, #935 ) ;
#6367 = CIRCLE ( 'NONE', #6013, 2.041999999999999815 ) ;
#6368 = ADVANCED_FACE ( 'NONE', ( #3907 ), #1760, .F. ) ;
#6369 = CARTESIAN_POINT ( 'NONE',  ( 386.6666666666666288, -20.00000000000000000, -159.8500000000001080 ) ) ;
#6370 = LINE ( 'NONE', #6408, #3412 ) ;
#6371 = CARTESIAN_POINT ( 'NONE',  ( 1.257172072275274388, -3.892973519170983110, -3.433252694550781303 ) ) ;
#6372 = LINE ( 'NONE', #197, #7237 ) ;
#6373 =( REPRESENTATION_RELATIONSHIP ('NONE','NONE', #5587, #5294 ) REPRESENTATION_RELATIONSHIP_WITH_TRANSFORMATION ( #3191 )SHAPE_REPRESENTATION_RELATIONSHIP( ) );
#6374 =( LENGTH_UNIT ( ) NAMED_UNIT ( * ) SI_UNIT ( .MILLI., .METRE. ) );
#6375 = ORIENTED_EDGE ( 'NONE', *, *, #5269, .T. ) ;
#6376 = EDGE_CURVE ( 'NONE', #4994, #1523, #5708, .T. ) ;
#6377 = CARTESIAN_POINT ( 'NONE',  ( 155.0000000000000000, 8.660254037844390851, 140.0000000000000000 ) ) ;
#6378 = ORIENTED_EDGE ( 'NONE', *, *, #3401, .T. ) ;
#6379 = CARTESIAN_POINT ( 'NONE',  ( 355.0000000000000000, 8.660254037844390851, 140.0000000000000000 ) ) ;
#6380 = CARTESIAN_POINT ( 'NONE',  ( -30.00000000000002842, -20.00000000000000000, -200.0000000000000000 ) ) ;
#6381 = DIRECTION ( 'NONE',  ( 1.000000000000000000, 0.000000000000000000, 0.000000000000000000 ) ) ;
#6382 = CARTESIAN_POINT ( 'NONE',  ( 2.500000000000000000, -2.357898499370432610, 3.252606517456513302E-15 ) ) ;
#6383 =( GEOMETRIC_REPRESENTATION_CONTEXT ( 3 ) GLOBAL_UNCERTAINTY_ASSIGNED_CONTEXT ( ( #4681 ) ) GLOBAL_UNIT_ASSIGNED_CONTEXT ( ( #3420, #1701, #2222 ) ) REPRESENTATION_CONTEXT ( 'NONE', 'WORKASPACE' ) );
#6384 = PLANE ( 'NONE',  #2781 ) ;
#6385 = PRODUCT_DEFINITION ( 'UNKNOWN', '', #3998, #5554 ) ;
#6386 = AXIS2_PLACEMENT_3D ( 'NONE', #5805, #4715, #119 ) ;
#6387 = ORIENTED_EDGE ( 'NONE', *, *, #4803, .F. ) ;
#6388 = PRODUCT_DEFINITION_FORMATION_WITH_SPECIFIED_SOURCE ( 'ANY', '', #7153, .NOT_KNOWN. ) ;
#6389 = ORIENTED_EDGE ( 'NONE', *, *, #2824, .F. ) ;
#6390 = VECTOR ( 'NONE', #3245, 1000.000000000000000 ) ;
#6391 = AXIS2_PLACEMENT_3D ( 'NONE', #4709, #1854, #4144 ) ;
#6392 = CARTESIAN_POINT ( 'NONE',  ( 45.00000000000000000, 8.660254037844390851, 140.0000000000000000 ) ) ;
#6393 = EDGE_LOOP ( 'NONE', ( #3095, #5584, #3597, #5115 ) ) ;
#6394 = PRESENTATION_STYLE_ASSIGNMENT (( #141 ) ) ;
#6395 = AXIS2_PLACEMENT_3D ( 'NONE', #2465, #1898, #4194 ) ;
#6396 = VECTOR ( 'NONE', #4569, 1000.000000000000000 ) ;
#6397 = CARTESIAN_POINT ( 'NONE',  ( -4.211399284164270895, 2.459729995988205964, -3.751162237960538715 ) ) ;
#6398 = VERTEX_POINT ( 'NONE', #2869 ) ;
#6399 = AXIS2_PLACEMENT_3D ( 'NONE', #5456, #4335, #3108 ) ;
#6400 = AXIS2_PLACEMENT_3D ( 'NONE', #3896, #1717, #5731 ) ;
#6401 = CARTESIAN_POINT ( 'NONE',  ( -2.000000000000006661, 3.464101615137750834, 0.000000000000000000 ) ) ;
#6402 = LINE ( 'NONE', #80, #6405 ) ;
#6403 = ADVANCED_FACE ( 'NONE', ( #6229 ), #3471, .F. ) ;
#6404 = VERTEX_POINT ( 'NONE', #5172 ) ;
#6405 = VECTOR ( 'NONE', #221, 1000.000000000000000 ) ;
#6406 = VERTEX_POINT ( 'NONE', #5112 ) ;
#6407 = CARTESIAN_POINT ( 'NONE',  ( 0.000000000000000000, 0.000000000000000000, -25.03750572909317285 ) ) ;
#6408 = CARTESIAN_POINT ( 'NONE',  ( 245.0000000000000000, 8.660254037844390851, 139.9990000000000236 ) ) ;
#6409 = VECTOR ( 'NONE', #5861, 1000.000000000000000 ) ;
#6410 = CARTESIAN_POINT ( 'NONE',  ( 4.141042297810615835, -2.227970268150433863, -3.687027686973623819 ) ) ;
#6411 = FACE_OUTER_BOUND ( 'NONE', #7335, .T. ) ;
#6412 = AXIS2_PLACEMENT_3D ( 'NONE', #2976, #691, #4583 ) ;
#6413 = FILL_AREA_STYLE_COLOUR ( '', #1144 ) ;
#6414 = ORIENTED_EDGE ( 'NONE', *, *, #3232, .T. ) ;
#6415 = DIRECTION ( 'NONE',  ( 1.000000000000000000, 0.000000000000000000, 0.000000000000000000 ) ) ;
#6416 = EDGE_CURVE ( 'NONE', #1142, #3012, #5661, .T. ) ;
#6417 = UNCERTAINTY_MEASURE_WITH_UNIT (LENGTH_MEASURE( 1.000000000000000082E-05 ), #4283, 'distance_accuracy_value', 'NONE');
#6418 = ORIENTED_EDGE ( 'NONE', *, *, #3562, .T. ) ;
#6419 = AXIS2_PLACEMENT_3D ( 'NONE', #2010, #2531, #5930 ) ;
#6420 = ORIENTED_EDGE ( 'NONE', *, *, #6796, .F. ) ;
#6421 =( REPRESENTATION_RELATIONSHIP ('NONE','NONE', #5587, #951 ) REPRESENTATION_RELATIONSHIP_WITH_TRANSFORMATION ( #2435 )SHAPE_REPRESENTATION_RELATIONSHIP( ) );
#6422 = DIRECTION ( 'NONE',  ( 0.000000000000000000, 0.000000000000000000, -1.000000000000000000 ) ) ;
#6423 = DIRECTION ( 'NONE',  ( 0.000000000000000000, 0.000000000000000000, 1.000000000000000000 ) ) ;
#6424 = LINE ( 'NONE', #1391, #6500 ) ;
#6425 = CARTESIAN_POINT ( 'NONE',  ( 1.800000000000002931, 0.000000000000000000, 0.000000000000000000 ) ) ;
#6426=STYLED_ITEM('',(#7439),#856);
#6427 = CARTESIAN_POINT ( 'NONE',  ( 1.567478505476134606E-15, 4.618802153517012066, -5.000000000000000000 ) ) ;
#6428 = ADVANCED_FACE ( 'NONE', ( #646 ), #7314, .F. ) ;
#6429 = ORIENTED_EDGE ( 'NONE', *, *, #3569, .F. ) ;
#6430 = ORIENTED_EDGE ( 'NONE', *, *, #6260, .F. ) ;
#6431 = CARTESIAN_POINT ( 'NONE',  ( 325.0000000000000000, 8.660254037844390851, 140.0000000000000000 ) ) ;
#6432 = ORIENTED_EDGE ( 'NONE', *, *, #3168, .T. ) ;
#6433 = DIRECTION ( 'NONE',  ( -1.000000000000000000, 0.000000000000000000, -0.000000000000000000 ) ) ;
#6434 = EDGE_LOOP ( 'NONE', ( #5655, #1578 ) ) ;
#6435 = CARTESIAN_POINT ( 'NONE',  ( 4.999999999999993783, 8.660254037844390851, -140.0000000000000000 ) ) ;
#6436 = CARTESIAN_POINT ( 'NONE',  ( 53.33333333333330017, -25.00000000000000000, 159.8500000000001080 ) ) ;
#6437 = CARTESIAN_POINT ( 'NONE',  ( 195.0000000000000000, 8.660254037844390851, 140.0000000000000000 ) ) ;
#6438 = SURFACE_STYLE_USAGE ( .BOTH. , #6958 ) ;
#6439 = ORIENTED_EDGE ( 'NONE', *, *, #1073, .T. ) ;
#6440 = EDGE_LOOP ( 'NONE', ( #6526, #4656, #6206, #5544 ) ) ;
#6441 = EDGE_CURVE ( 'NONE', #7192, #6404, #4542, .T. ) ;
#6442 = FACE_OUTER_BOUND ( 'NONE', #991, .T. ) ;
#6443 = CONTEXT_DEPENDENT_SHAPE_REPRESENTATION ( #3933, #3039 ) ;
#6444 = DIRECTION ( 'NONE',  ( -0.000000000000000000, 0.000000000000000000, 1.000000000000000000 ) ) ;
#6445 = CARTESIAN_POINT ( 'NONE',  ( 25.00000000000000000, 0.000000000000000000, 0.000000000000000000 ) ) ;
#6446 = EDGE_LOOP ( 'NONE', ( #1691, #2997, #2148, #3679 ) ) ;
#6447 = CARTESIAN_POINT ( 'NONE',  ( -0.6920835326022555245, -4.454600218803899558, -3.597382984111586079 ) ) ;
#6448 = ORIENTED_EDGE ( 'NONE', *, *, #1808, .T. ) ;
#6449 = EDGE_LOOP ( 'NONE', ( #4460, #5604, #6639, #4169 ) ) ;
#6450 = CARTESIAN_POINT ( 'NONE',  ( 325.0000000000000000, -8.660254037844389075, 145.0000000000000284 ) ) ;
#6451 = CARTESIAN_POINT ( 'NONE',  ( -3.453038570459499024, -2.625189405340453419, -3.535263753545272891 ) ) ;
#6452 = CARTESIAN_POINT ( 'NONE',  ( 84.99999999999998579, 8.660254037844390851, 145.0000000000000284 ) ) ;
#6453 = CARTESIAN_POINT ( 'NONE',  ( 0.000000000000000000, -1.178949249685213863, 2.042000000000002924 ) ) ;
#6454 = EDGE_CURVE ( 'NONE', #2630, #5914, #4607, .T. ) ;
#6455 = EDGE_CURVE ( 'NONE', #1325, #7192, #4465, .T. ) ;
#6456 = CYLINDRICAL_SURFACE ( 'NONE', #6977, 2.649999999999985700 ) ;
#6457 = DIRECTION ( 'NONE',  ( 0.000000000000000000, 0.000000000000000000, -1.000000000000000000 ) ) ;
#6458 = EDGE_LOOP ( 'NONE', ( #827, #46, #3919, #3576 ) ) ;
#6459 = ORIENTED_EDGE ( 'NONE', *, *, #2636, .F. ) ;
#6460 = ITEM_DEFINED_TRANSFORMATION ( 'NONE', 'NONE', #186,  #1963 ) ;
#6461 = DIRECTION ( 'NONE',  ( 1.000000000000000000, 0.000000000000000000, 0.000000000000000000 ) ) ;
#6462 = ORIENTED_EDGE ( 'NONE', *, *, #5739, .T. ) ;
#6463 = ADVANCED_FACE ( 'NONE', ( #1235 ), #3021, .T. ) ;
#6464 =( NAMED_UNIT ( * ) PLANE_ANGLE_UNIT ( ) SI_UNIT ( $, .RADIAN. ) );
#6465 = EDGE_CURVE ( 'NONE', #1782, #183, #3506, .T. ) ;
#6466 = CARTESIAN_POINT ( 'NONE',  ( -4.000000000000000000, 2.511478553582031203, -3.469254451724764543 ) ) ;
#6467 = UNCERTAINTY_MEASURE_WITH_UNIT (LENGTH_MEASURE( 1.000000000000000082E-05 ), #3830, 'distance_accuracy_value', 'NONE');
#6468 = TOROIDAL_SURFACE ( 'NONE', #7177, 10.20000000000000107, 0.2000000000000031197 ) ;
#6469 = VERTEX_POINT ( 'NONE', #3541 ) ;
#6470 = EDGE_LOOP ( 'NONE', ( #6018, #5365, #928, #3770 ) ) ;
#6471 = LINE ( 'NONE', #1226, #5568 ) ;
#6472=STYLED_ITEM('',(#7432),#794);
#6473 = LINE ( 'NONE', #1330, #4478 ) ;
#6474 = PRODUCT_DEFINITION_SHAPE ( 'NONE', 'NONE',  #7373 ) ;
#6475 = CARTESIAN_POINT ( 'NONE',  ( 2.000000000000001776, 1.524685264938454646E-15, 12.44999999999999929 ) ) ;
#6476 = VERTEX_POINT ( 'NONE', #685 ) ;
#6477 = AXIS2_PLACEMENT_3D ( 'NONE', #1389, #7048, #1280 ) ;
#6478 = ADVANCED_FACE ( 'NONE', ( #5239 ), #5810, .F. ) ;
#6479 = CARTESIAN_POINT ( 'NONE',  ( -20.63749999999999929, 1.313433692085536673E-15, 10.72500000000000142 ) ) ;
#6480 = DIRECTION ( 'NONE',  ( 0.000000000000000000, 0.000000000000000000, 1.000000000000000000 ) ) ;
#6481 = CARTESIAN_POINT ( 'NONE',  ( 0.000000000000000000, 0.000000000000000000, 140.0000000000000000 ) ) ;
#6482 = CARTESIAN_POINT ( 'NONE',  ( 0.000000000000000000, 0.000000000000000000, 0.000000000000000000 ) ) ;
#6483 = ORIENTED_EDGE ( 'NONE', *, *, #4163, .T. ) ;
#6484 = VECTOR ( 'NONE', #4418, 1000.000000000000000 ) ;
#6485 = ORIENTED_EDGE ( 'NONE', *, *, #5366, .T. ) ;
#6486 = EDGE_LOOP ( 'NONE', ( #6226, #4036 ) ) ;
#6487 = CARTESIAN_POINT ( 'NONE',  ( 4.000000000000000888, 1.539600717838996990, -3.300726591567079815 ) ) ;
#6488 = DIRECTION ( 'NONE',  ( 1.000000000000000000, 0.000000000000000000, 0.000000000000000000 ) ) ;
#6489 = CARTESIAN_POINT ( 'NONE',  ( 4.211140560182196957, 2.431303136016536470, -3.745885042887433514 ) ) ;
#6490 = CARTESIAN_POINT ( 'NONE',  ( 195.0000000000000000, -8.660254037844389075, 145.0000000000000284 ) ) ;
#6491 = CIRCLE ( 'NONE', #6253, 0.2500000000000002220 ) ;
#6492 = DIRECTION ( 'NONE',  ( 1.000000000000000000, 0.000000000000000000, 0.000000000000000000 ) ) ;
#6493 = EDGE_CURVE ( 'NONE', #1972, #3032, #6372, .T. ) ;
#6494 = DIRECTION ( 'NONE',  ( 1.000000000000000000, 0.000000000000000000, 0.000000000000000000 ) ) ;
#6495 = ADVANCED_FACE ( 'NONE', ( #123 ), #2377, .T. ) ;
#6496 = ORIENTED_EDGE ( 'NONE', *, *, #1263, .F. ) ;
#6497 = VECTOR ( 'NONE', #5564, 1000.000000000000000 ) ;
#6498 = DIRECTION ( 'NONE',  ( -0.000000000000000000, -0.000000000000000000, -1.000000000000000000 ) ) ;
#6499 = ORIENTED_EDGE ( 'NONE', *, *, #3521, .F. ) ;
#6500 = VECTOR ( 'NONE', #2429, 1000.000000000000000 ) ;
#6501 = DIRECTION ( 'NONE',  ( 6.123233995736766036E-17, -1.000000000000000000, 0.000000000000000000 ) ) ;
#6502 = FACE_BOUND ( 'NONE', #5653, .T. ) ;
#6503 = VECTOR ( 'NONE', #4311, 1000.000000000000000 ) ;
#6504 = ADVANCED_FACE ( 'NONE', ( #6411 ), #1303, .T. ) ;
#6505 = ORIENTED_EDGE ( 'NONE', *, *, #462, .F. ) ;
#6506 = EDGE_LOOP ( 'NONE', ( #1956, #2606, #6211, #3384, #6626 ) ) ;
#6507 = DIRECTION ( 'NONE',  ( -0.000000000000000000, -0.000000000000000000, 1.000000000000000000 ) ) ;
#6508 = AXIS2_PLACEMENT_3D ( 'NONE', #5326, #4763, #1349 ) ;
#6509 = DIRECTION ( 'NONE',  ( -0.000000000000000000, 1.000000000000000000, 0.000000000000000000 ) ) ;
#6510 = ORIENTED_EDGE ( 'NONE', *, *, #3338, .F. ) ;
#6511 = CARTESIAN_POINT ( 'NONE',  ( 275.0000000000000000, 8.660254037844390851, 140.0000000000000000 ) ) ;
#6512 =( REPRESENTATION_RELATIONSHIP ('NONE','NONE', #5587, #5294 ) REPRESENTATION_RELATIONSHIP_WITH_TRANSFORMATION ( #3892 )SHAPE_REPRESENTATION_RELATIONSHIP( ) );
#6513 = EDGE_CURVE ( 'NONE', #2826, #767, #4678, .T. ) ;
#6514 = AXIS2_PLACEMENT_3D ( 'NONE', #230, #4646, #160 ) ;
#6515 = ORIENTED_EDGE ( 'NONE', *, *, #2140, .T. ) ;
#6516 = STYLED_ITEM ( 'NONE', ( #6394 ), #402 ) ;
#6517 = CARTESIAN_POINT ( 'NONE',  ( 303.3333333333333144, -20.00000000000000000, -162.5000000000000853 ) ) ;
#6518 = ITEM_DEFINED_TRANSFORMATION ( 'NONE', 'NONE', #4590,  #1963 ) ;
#6519 = CARTESIAN_POINT ( 'NONE',  ( 0.000000000000000000, 0.000000000000000000, 0.000000000000000000 ) ) ;
#6520 = CARTESIAN_POINT ( 'NONE',  ( -20.63749999999999574, 0.000000000000000000, 0.000000000000000000 ) ) ;
#6521 = CARTESIAN_POINT ( 'NONE',  ( 0.000000000000000000, 0.000000000000000000, 0.000000000000000000 ) ) ;
#6522 = ORIENTED_EDGE ( 'NONE', *, *, #1872, .T. ) ;
#6523 = PLANE ( 'NONE',  #7094 ) ;
#6524 = EDGE_LOOP ( 'NONE', ( #3048, #3755 ) ) ;
#6525 = AXIS2_PLACEMENT_3D ( 'NONE', #4928, #7107, #5448 ) ;
#6526 = ORIENTED_EDGE ( 'NONE', *, *, #6750, .F. ) ;
#6527 = DIRECTION ( 'NONE',  ( -0.000000000000000000, -0.000000000000000000, -1.000000000000000000 ) ) ;
#6528 = CIRCLE ( 'NONE', #7002, 10.00000000000000000 ) ;
#6529 = DIRECTION ( 'NONE',  ( 0.000000000000000000, 1.000000000000000000, -1.224646799147353207E-16 ) ) ;
#6530 = CARTESIAN_POINT ( 'NONE',  ( 4.154306624731137099, 2.398490048084935822, -3.721999068284414847 ) ) ;
#6531 = DIRECTION ( 'NONE',  ( -1.000000000000000000, 0.000000000000000000, 0.000000000000000000 ) ) ;
#6532 = DIRECTION ( 'NONE',  ( -0.000000000000000000, 1.000000000000000000, -0.000000000000000000 ) ) ;
#6533 = DIRECTION ( 'NONE',  ( 1.000000000000000000, 0.000000000000000000, 0.000000000000000000 ) ) ;
#6534 = ORIENTED_EDGE ( 'NONE', *, *, #6101, .F. ) ;
#6535 = DIRECTION ( 'NONE',  ( -1.000000000000000000, -0.000000000000000000, -0.000000000000000000 ) ) ;
#6536 = ORIENTED_EDGE ( 'NONE', *, *, #5900, .T. ) ;
#6537 = EDGE_CURVE ( 'NONE', #3857, #5460, #5843, .T. ) ;
#6538 = DIRECTION ( 'NONE',  ( -1.000000000000000000, 0.000000000000000000, 0.000000000000000000 ) ) ;
#6539 = VECTOR ( 'NONE', #5984, 1000.000000000000000 ) ;
#6540 = SHAPE_REPRESENTATION_RELATIONSHIP ( 'NONE' , 'NONE' ,  #3270, #5754 ) ;
#6541 = DIRECTION ( 'NONE',  ( 0.000000000000000000, 0.000000000000000000, 1.000000000000000000 ) ) ;
#6542 = ORIENTED_EDGE ( 'NONE', *, *, #3949, .F. ) ;
#6543 = EDGE_LOOP ( 'NONE', ( #6902, #4588, #7117, #330 ) ) ;
#6544 = CARTESIAN_POINT ( 'NONE',  ( 1.312671235360372224, 3.860931062424219462, -0.05923475698270440348 ) ) ;
#6545=STYLED_ITEM('',(#7446),#5701);
#6546 = CARTESIAN_POINT ( 'NONE',  ( -4.211140560182196957, -2.431303136016552013, -3.745885042887436178 ) ) ;
#6547 = EDGE_CURVE ( 'NONE', #1550, #4157, #5315, .T. ) ;
#6548 = DIRECTION ( 'NONE',  ( -0.000000000000000000, -0.000000000000000000, 1.000000000000000000 ) ) ;
#6549 = ORIENTED_EDGE ( 'NONE', *, *, #2497, .F. ) ;
#6550 = DIRECTION ( 'NONE',  ( 1.000000000000000000, 0.000000000000000000, 0.000000000000000000 ) ) ;
#6551 = CONTEXT_DEPENDENT_SHAPE_REPRESENTATION ( #1250, #616 ) ;
#6552 = DIRECTION ( 'NONE',  ( -1.000000000000000000, 0.000000000000000000, 0.000000000000000000 ) ) ;
#6553 = FACE_BOUND ( 'NONE', #1893, .T. ) ;
#6554 = EDGE_CURVE ( 'NONE', #563, #2492, #1732, .T. ) ;
#6555 = DIRECTION ( 'NONE',  ( 0.000000000000000000, 0.000000000000000000, 1.000000000000000000 ) ) ;
#6556 = EDGE_LOOP ( 'NONE', ( #3490, #6536 ) ) ;
#6557 = DIRECTION ( 'NONE',  ( 0.000000000000000000, 1.000000000000000000, 0.000000000000000000 ) ) ;
#6558 = PRODUCT_DEFINITION_SHAPE ( 'NONE', 'NONE',  #7365 ) ;
#6559 = EDGE_CURVE ( 'NONE', #1304, #7016, #2968, .T. ) ;
#6560 = AXIS2_PLACEMENT_3D ( 'NONE', #845, #3224, #6669 ) ;
#6561 = VERTEX_POINT ( 'NONE', #3005 ) ;
#6562 = ORIENTED_EDGE ( 'NONE', *, *, #7297, .T. ) ;
#6563 = CARTESIAN_POINT ( 'NONE',  ( -1.799999999999996048, 0.000000000000000000, 0.000000000000000000 ) ) ;
#6564 = CARTESIAN_POINT ( 'NONE',  ( 386.6666666666666288, -14.99999999999999822, 159.8500000000001080 ) ) ;
#6565 = CARTESIAN_POINT ( 'NONE',  ( -4.211140560182196957, 2.431303136016537803, -3.745885042887433514 ) ) ;
#6566 = CARTESIAN_POINT ( 'NONE',  ( 24.55500000000002103, 3.061616997868384620E-16, -2.500000000000001332 ) ) ;
#6567 = FACE_OUTER_BOUND ( 'NONE', #4433, .T. ) ;
#6568 = CARTESIAN_POINT ( 'NONE',  ( -13.50000000000000000, 0.000000000000000000, -121.0000000000000000 ) ) ;
#6569 = ORIENTED_EDGE ( 'NONE', *, *, #4171, .F. ) ;
#6570 = CARTESIAN_POINT ( 'NONE',  ( 53.33333333333330017, -20.00000000000000000, -165.1500000000000625 ) ) ;
#6571 = CARTESIAN_POINT ( 'NONE',  ( 2.804994570502171047, 3.229033611042449792, -3.526374918436834704 ) ) ;
#6572 = ORIENTED_EDGE ( 'NONE', *, *, #556, .T. ) ;
#6573 = FACE_BOUND ( 'NONE', #561, .T. ) ;
#6574 = EDGE_CURVE ( 'NONE', #6247, #468, #4486, .T. ) ;
#6575 = ORIENTED_EDGE ( 'NONE', *, *, #3562, .F. ) ;
#6576 = ORIENTED_EDGE ( 'NONE', *, *, #3209, .F. ) ;
#6577 = FACE_OUTER_BOUND ( 'NONE', #3685, .T. ) ;
#6578 = VECTOR ( 'NONE', #15, 1000.000000000000000 ) ;
#6579 = CARTESIAN_POINT ( 'NONE',  ( 136.6666666666666288, -14.99999999999999822, 165.1500000000000625 ) ) ;
#6580 = CYLINDRICAL_SURFACE ( 'NONE', #2105, 2.649999999999985700 ) ;
#6581 = EDGE_CURVE ( 'NONE', #4993, #153, #891, .T. ) ;
#6582 = EDGE_LOOP ( 'NONE', ( #1668, #3938, #2026, #3097 ) ) ;
#6583 = EDGE_CURVE ( 'NONE', #6697, #2874, #4785, .T. ) ;
#6584 = DIRECTION ( 'NONE',  ( -0.000000000000000000, -0.000000000000000000, -1.000000000000000000 ) ) ;
#6585 = CARTESIAN_POINT ( 'NONE',  ( 195.0000000000000000, -8.660254037844389075, 140.0000000000000000 ) ) ;
#6586 = DIRECTION ( 'NONE',  ( -0.000000000000000000, 1.000000000000000000, -0.000000000000000000 ) ) ;
#6587 = DIRECTION ( 'NONE',  ( 0.000000000000000000, 0.000000000000000000, 1.000000000000000000 ) ) ;
#6588 = ORIENTED_EDGE ( 'NONE', *, *, #3894, .F. ) ;
#6589 = DIRECTION ( 'NONE',  ( 0.000000000000000000, 0.000000000000000000, -1.000000000000000000 ) ) ;
#6590 = CONICAL_SURFACE ( 'NONE', #5509, 4.000000000000000000, 0.8911886515913786111 ) ;
#6591 = ADVANCED_FACE ( 'NONE', ( #745 ), #6934, .T. ) ;
#6592 = EDGE_LOOP ( 'NONE', ( #2128, #220 ) ) ;
#6593 = PRODUCT_DEFINITION_CONTEXT ( 'detailed design', #6186, 'design' ) ;
#6594 = ORIENTED_EDGE ( 'NONE', *, *, #5103, .T. ) ;
#6595 = CARTESIAN_POINT ( 'NONE',  ( 35.00000000000000000, -8.660254037844389075, 145.0000000000000284 ) ) ;
#6596 = CARTESIAN_POINT ( 'NONE',  ( -2.742827927723112236, -3.035229711105190464, -3.433252694550595230 ) ) ;
#6597 = DIRECTION ( 'NONE',  ( 0.000000000000000000, 0.000000000000000000, 1.000000000000000000 ) ) ;
#6598 = CARTESIAN_POINT ( 'NONE',  ( 25.00000000000000000, 0.000000000000000000, 0.000000000000000000 ) ) ;
#6599 = ADVANCED_FACE ( 'NONE', ( #7041 ), #4223, .T. ) ;
#6600 = B_SPLINE_CURVE_WITH_KNOTS ( 'NONE', 3,
 ( #6277, #2321, #4623, #3948, #6345, #1145 ),
 .UNSPECIFIED., .F., .F.,
 ( 4, 2, 4 ),
 ( 0.002365888236227967761, 0.003551327329835077609, 0.004736766423442186590 ),
 .UNSPECIFIED. ) ;
#6601 = FACE_OUTER_BOUND ( 'NONE', #3934, .T. ) ;
#6602 = DIRECTION ( 'NONE',  ( 0.000000000000000000, 0.000000000000000000, -1.000000000000000000 ) ) ;
#6603 = ORIENTED_EDGE ( 'NONE', *, *, #6062, .F. ) ;
#6604 = AXIS2_PLACEMENT_3D ( 'NONE', #2276, #1657, #3942 ) ;
#6605 = CARTESIAN_POINT ( 'NONE',  ( 75.00000000000001421, -8.660254037844389075, 139.9990000000000236 ) ) ;
#6606 = CARTESIAN_POINT ( 'NONE',  ( 386.6666666666666288, -20.00000000000000000, 159.8500000000001080 ) ) ;
#6607 = ORIENTED_EDGE ( 'NONE', *, *, #2473, .F. ) ;
#6608 = AXIS2_PLACEMENT_3D ( 'NONE', #4332, #7184, #2000 ) ;
#6609 = CARTESIAN_POINT ( 'NONE',  ( 0.7826237921249276086, 0.000000000000000000, 12.44999999999999929 ) ) ;
#6610 =( NAMED_UNIT ( * ) PLANE_ANGLE_UNIT ( ) SI_UNIT ( $, .RADIAN. ) );
#6611 =( REPRESENTATION_RELATIONSHIP ('NONE','NONE', #5587, #3270 ) REPRESENTATION_RELATIONSHIP_WITH_TRANSFORMATION ( #7056 )SHAPE_REPRESENTATION_RELATIONSHIP( ) );
#6612 = DIRECTION ( 'NONE',  ( -0.000000000000000000, 1.000000000000000000, 0.000000000000000000 ) ) ;
#6613 = EDGE_CURVE ( 'NONE', #1004, #7081, #5796, .T. ) ;
#6614 = FACE_OUTER_BOUND ( 'NONE', #1669, .T. ) ;
#6615 = AXIS2_PLACEMENT_3D ( 'NONE', #1790, #1863, #4154 ) ;
#6616 = ORIENTED_EDGE ( 'NONE', *, *, #728, .T. ) ;
#6617 = DIRECTION ( 'NONE',  ( 0.000000000000000000, 0.000000000000000000, 1.000000000000000000 ) ) ;
#6618 = VERTEX_POINT ( 'NONE', #6035 ) ;
#6619 = PRODUCT_DEFINITION_SHAPE ( 'NONE', 'NONE',  #7347 ) ;
#6620 = CARTESIAN_POINT ( 'NONE',  ( -4.101948962585905356, -2.368261337751088824, -3.681124513963624167 ) ) ;
#6621 = VECTOR ( 'NONE', #172, 1000.000000000000000 ) ;
#6622 = AXIS2_PLACEMENT_3D ( 'NONE', #6521, #198, #231 ) ;
#6623 = AXIS2_PLACEMENT_3D ( 'NONE', #3167, #4398, #2700 ) ;
#6624 = DIRECTION ( 'NONE',  ( -0.000000000000000000, 1.000000000000000000, -0.000000000000000000 ) ) ;
#6625 = CARTESIAN_POINT ( 'NONE',  ( 205.0000000000000284, 8.660254037844390851, 140.0000000000000000 ) ) ;
#6626 = ORIENTED_EDGE ( 'NONE', *, *, #3578, .T. ) ;
#6627 = AXIS2_PLACEMENT_3D ( 'NONE', #3262, #452, #2226 ) ;
#6628 = VECTOR ( 'NONE', #3204, 1000.000000000000000 ) ;
#6629 = AXIS2_PLACEMENT_3D ( 'NONE', #1660, #4618, #2811 ) ;
#6630 = CARTESIAN_POINT ( 'NONE',  ( 0.000000000000000000, -2.357898499370432610, 3.252606517456513302E-15 ) ) ;
#6631 = ADVANCED_FACE ( 'NONE', ( #3811 ), #4821, .F. ) ;
#6632 = CARTESIAN_POINT ( 'NONE',  ( 0.000000000000000000, 0.000000000000000000, -140.0000000000000000 ) ) ;
#6633 = CARTESIAN_POINT ( 'NONE',  ( 386.6666666666666288, -30.00000000000000355, 162.5000000000000853 ) ) ;
#6634 = ORIENTED_EDGE ( 'NONE', *, *, #5680, .F. ) ;
#6635 = VECTOR ( 'NONE', #659, 1000.000000000000000 ) ;
#6636 = CARTESIAN_POINT ( 'NONE',  ( -1.747541505913277282, 3.837784562140256650, -3.503702292528906526 ) ) ;
#6637 = VECTOR ( 'NONE', #6053, 1000.000000000000000 ) ;
#6638 = ORIENTED_EDGE ( 'NONE', *, *, #2459, .T. ) ;
#6639 = ORIENTED_EDGE ( 'NONE', *, *, #920, .F. ) ;
#6640 = CARTESIAN_POINT ( 'NONE',  ( 4.000000000000000000, -1.942223658245635809, -0.3516579909967643691 ) ) ;
#6641 = DIRECTION ( 'NONE',  ( -0.000000000000000000, 1.000000000000000000, -0.000000000000000000 ) ) ;
#6642 = CIRCLE ( 'NONE', #4370, 13.50000000000000000 ) ;
#6643 = AXIS2_PLACEMENT_3D ( 'NONE', #2564, #4298, #342 ) ;
#6644 = DIRECTION ( 'NONE',  ( 0.000000000000000000, 0.000000000000000000, -1.000000000000000000 ) ) ;
#6645 = LINE ( 'NONE', #6049, #5420 ) ;
#6646 = ADVANCED_FACE ( 'NONE', ( #7113 ), #1970, .F. ) ;
#6647 = DIRECTION ( 'NONE',  ( -0.000000000000000000, -0.000000000000000000, 1.000000000000000000 ) ) ;
#6648 = CYLINDRICAL_SURFACE ( 'NONE', #1603, 2.649999999999985700 ) ;
#6649 = DIRECTION ( 'NONE',  ( 0.000000000000000000, 0.000000000000000000, 1.000000000000000000 ) ) ;
#6650 = AXIS2_PLACEMENT_3D ( 'NONE', #1487, #1157, #5608 ) ;
#6651 = VERTEX_POINT ( 'NONE', #4419 ) ;
#6652 = CIRCLE ( 'NONE', #1965, 2.649999999999985700 ) ;
#6653 = DIRECTION ( 'NONE',  ( 0.000000000000000000, -0.000000000000000000, 1.000000000000000000 ) ) ;
#6654 = CARTESIAN_POINT ( 'NONE',  ( 5.200000000000002842, 0.000000000000000000, 0.000000000000000000 ) ) ;
#6655 = LINE ( 'NONE', #2620, #6720 ) ;
#6656 =( NAMED_UNIT ( * ) PLANE_ANGLE_UNIT ( ) SI_UNIT ( $, .RADIAN. ) );
#6657 = EDGE_CURVE ( 'NONE', #5543, #807, #5092, .T. ) ;
#6658 = AXIS2_PLACEMENT_3D ( 'NONE', #5501, #2731, #3819 ) ;
#6659 = CARTESIAN_POINT ( 'NONE',  ( 114.9999999999999858, 8.660254037844390851, 139.9990000000000236 ) ) ;
#6660 = CARTESIAN_POINT ( 'NONE',  ( 164.9999999999999716, 8.660254037844390851, 145.0000000000000284 ) ) ;
#6661 = EDGE_LOOP ( 'NONE', ( #502, #486, #3680, #6496 ) ) ;
#6663 = CIRCLE ( 'NONE', #1046, 10.20000000000000107 ) ;
#6662 = DIRECTION ( 'NONE',  ( 1.000000000000000000, 0.000000000000000000, 0.000000000000000000 ) ) ;
#6664 = ORIENTED_EDGE ( 'NONE', *, *, #1816, .T. ) ;
#6665 =( REPRESENTATION_RELATIONSHIP ('NONE','NONE', #5587, #5294 ) REPRESENTATION_RELATIONSHIP_WITH_TRANSFORMATION ( #3003 )SHAPE_REPRESENTATION_RELATIONSHIP( ) );
#6666 = PRODUCT_DEFINITION ( 'UNKNOWN', '', #3872, #6080 ) ;
#6667 = DIRECTION ( 'NONE',  ( -1.000000000000000000, 1.224646799147352714E-16, 0.000000000000000000 ) ) ;
#6668 = VECTOR ( 'NONE', #110, 1000.000000000000000 ) ;
#6669 = DIRECTION ( 'NONE',  ( 0.000000000000000000, 0.000000000000000000, -1.000000000000000000 ) ) ;
#6670 = DIRECTION ( 'NONE',  ( -0.000000000000000000, -0.000000000000000000, 1.000000000000000000 ) ) ;
#6671 = VERTEX_POINT ( 'NONE', #2562 ) ;
#6672 = CYLINDRICAL_SURFACE ( 'NONE', #5399, 9.999999999999996447 ) ;
#6673 = DIRECTION ( 'NONE',  ( -0.000000000000000000, 0.000000000000000000, 1.000000000000000000 ) ) ;
#6674 = DIRECTION ( 'NONE',  ( 0.000000000000000000, 0.000000000000000000, 1.000000000000000000 ) ) ;
#6675 = DIRECTION ( 'NONE',  ( 0.000000000000000000, 0.000000000000000000, 1.000000000000000000 ) ) ;
#6676 = ORIENTED_EDGE ( 'NONE', *, *, #288, .T. ) ;
#6677 = DIRECTION ( 'NONE',  ( 0.000000000000000000, -0.000000000000000000, 1.000000000000000000 ) ) ;
#6678 = ADVANCED_FACE ( 'NONE', ( #7226 ), #3271, .T. ) ;
#6679 = ORIENTED_EDGE ( 'NONE', *, *, #3332, .T. ) ;
#6680 = ORIENTED_EDGE ( 'NONE', *, *, #5834, .T. ) ;
#6681 = DIRECTION ( 'NONE',  ( 1.000000000000000000, 0.000000000000000000, 0.000000000000000000 ) ) ;
#6682 = DIRECTION ( 'NONE',  ( 0.000000000000000000, 0.000000000000000000, 1.000000000000000000 ) ) ;
#6683 = CONTEXT_DEPENDENT_SHAPE_REPRESENTATION ( #2378, #281 ) ;
#6684 = CARTESIAN_POINT ( 'NONE',  ( 2.855764796983346177, -2.970025579236428737, -0.09382832055446485575 ) ) ;
#6685 = CARTESIAN_POINT ( 'NONE',  ( 0.000000000000000000, 0.000000000000000000, 0.000000000000000000 ) ) ;
#6686 = CARTESIAN_POINT ( 'NONE',  ( 53.33333333333330017, -15.00000000000000000, 162.5000000000000853 ) ) ;
#6687 = CARTESIAN_POINT ( 'NONE',  ( 2.500000000000000000, 3.004629197474318851E-15, 2.042000000000000259 ) ) ;
#6688 = ORIENTED_EDGE ( 'NONE', *, *, #1661, .F. ) ;
#6689 = EDGE_CURVE ( 'NONE', #3129, #7309, #1022, .T. ) ;
#6690 = CARTESIAN_POINT ( 'NONE',  ( 2.000000000000008882, 3.464101615137749945, 0.000000000000000000 ) ) ;
#6691 = CARTESIAN_POINT ( 'NONE',  ( -2.500000000000000888, 0.000000000000000000, -4.974599999999998801 ) ) ;
#6692 = CARTESIAN_POINT ( 'NONE',  ( 2.000000000000008882, 3.464101615137749945, 0.000000000000000000 ) ) ;
#6693 = ADVANCED_FACE ( 'NONE', ( #6111 ), #3851, .F. ) ;
#6694 =( NAMED_UNIT ( * ) PLANE_ANGLE_UNIT ( ) SI_UNIT ( $, .RADIAN. ) );
#6695 = DIRECTION ( 'NONE',  ( 0.000000000000000000, 0.000000000000000000, -1.000000000000000000 ) ) ;
#6696 = CARTESIAN_POINT ( 'NONE',  ( 5.200000000000002842, 0.000000000000000000, 2.500000000000000888 ) ) ;
#6697 = VERTEX_POINT ( 'NONE', #3193 ) ;
#6698 = ORIENTED_EDGE ( 'NONE', *, *, #3496, .T. ) ;
#6699 = EDGE_CURVE ( 'NONE', #4862, #3982, #897, .T. ) ;
#6700 = CARTESIAN_POINT ( 'NONE',  ( 320.0000000000000000, 0.000000000000000000, 0.000000000000000000 ) ) ;
#6701 = VERTEX_POINT ( 'NONE', #7187 ) ;
#6702 = DIRECTION ( 'NONE',  ( -1.000000000000000000, 0.000000000000000000, 0.000000000000000000 ) ) ;
#6703 = LINE ( 'NONE', #3267, #5542 ) ;
#6704 = DIRECTION ( 'NONE',  ( -0.000000000000000000, 1.000000000000000000, -0.000000000000000000 ) ) ;
#6705 = ORIENTED_EDGE ( 'NONE', *, *, #717, .F. ) ;
#6706 = CARTESIAN_POINT ( 'NONE',  ( 5.200000000000002842, 0.000000000000000000, 0.000000000000000000 ) ) ;
#6707 = DIRECTION ( 'NONE',  ( 0.000000000000000000, 0.000000000000000000, -1.000000000000000000 ) ) ;
#6708 = DIRECTION ( 'NONE',  ( 0.000000000000000000, 0.000000000000000000, -1.000000000000000000 ) ) ;
#6709 = AXIS2_PLACEMENT_3D ( 'NONE', #3537, #4675, #5203 ) ;
#6710 = CARTESIAN_POINT ( 'NONE',  ( 136.6666666666666288, -30.00000000000000355, 162.5000000000000853 ) ) ;
#6711 = ORIENTED_EDGE ( 'NONE', *, *, #6796, .T. ) ;
#6712 = FACE_BOUND ( 'NONE', #7191, .T. ) ;
#6713 = ADVANCED_FACE ( 'NONE', ( #6553, #974, #4859, #1417, #3690, #3078, #5379, #264, #1535, #3231, #4297, #377, #5991 ), #3156, .T. ) ;
#6714 = VERTEX_POINT ( 'NONE', #5417 ) ;
#6715 = ORIENTED_EDGE ( 'NONE', *, *, #2995, .T. ) ;
#6716 = CARTESIAN_POINT ( 'NONE',  ( 395.0000000000000000, -8.660254037844389075, 145.0000000000000284 ) ) ;
#6717 = FACE_OUTER_BOUND ( 'NONE', #4407, .T. ) ;
#6718 = LINE ( 'NONE', #2573, #5173 ) ;
#6719 = CARTESIAN_POINT ( 'NONE',  ( 124.9999999999999858, -8.660254037844389075, 139.9990000000000236 ) ) ;
#6720 = VECTOR ( 'NONE', #4920, 1000.000000000000000 ) ;
#6721 = VECTOR ( 'NONE', #6381, 1000.000000000000000 ) ;
#6722 = MECHANICAL_DESIGN_GEOMETRIC_PRESENTATION_REPRESENTATION (  '', ( #6472 ), #3911 ) ;
#6723 = PLANE ( 'NONE',  #650 ) ;
#6724 = CARTESIAN_POINT ( 'NONE',  ( 2.000000000000005329, -3.464101615137751722, 0.000000000000000000 ) ) ;
#6725 = VERTEX_POINT ( 'NONE', #304 ) ;
#6726 = DIRECTION ( 'NONE',  ( -0.000000000000000000, -0.000000000000000000, -1.000000000000000000 ) ) ;
#6727 = CARTESIAN_POINT ( 'NONE',  ( 219.9999999999999716, -20.00000000000000000, 162.5000000000000853 ) ) ;
#6728 = CARTESIAN_POINT ( 'NONE',  ( -2.688821387764050996E-14, -4.618802153517012954, -0.4999999999999995559 ) ) ;
#6729 = LINE ( 'NONE', #1630, #1212 ) ;
#6730 = EDGE_CURVE ( 'NONE', #3050, #3261, #2640, .T. ) ;
#6731 = PRESENTATION_STYLE_ASSIGNMENT (( #5010 ) ) ;
#6732 = ADVANCED_FACE ( 'NONE', ( #1496 ), #5533, .F. ) ;
#6733 = AXIS2_PLACEMENT_3D ( 'NONE', #4211, #253, #1407 ) ;
#6734 = EDGE_LOOP ( 'NONE', ( #476, #217, #942, #174 ) ) ;
#6735 = VERTEX_POINT ( 'NONE', #424 ) ;
#6736 = VECTOR ( 'NONE', #6856, 1000.000000000000000 ) ;
#6737 = DIRECTION ( 'NONE',  ( 0.000000000000000000, 0.000000000000000000, 1.000000000000000000 ) ) ;
#6738 = ORIENTED_EDGE ( 'NONE', *, *, #4078, .T. ) ;
#6739 = CARTESIAN_POINT ( 'NONE',  ( 53.33333333333330017, -20.00000000000000000, 159.8500000000001080 ) ) ;
#6740 = AXIS2_PLACEMENT_3D ( 'NONE', #7050, #723, #2977 ) ;
#6741 = EDGE_CURVE ( 'NONE', #3920, #584, #1713, .T. ) ;
#6742 = PLANE ( 'NONE',  #5084 ) ;
#6743 = LINE ( 'NONE', #1640, #7021 ) ;
#6744 = VERTEX_POINT ( 'NONE', #6857 ) ;
#6745 = CARTESIAN_POINT ( 'NONE',  ( 315.0000000000000568, -8.660254037844389075, 145.0000000000000284 ) ) ;
#6746=STYLED_ITEM('',(#7432),#3126);
#6747 = DIRECTION ( 'NONE',  ( -1.000000000000000000, 0.000000000000000000, 0.000000000000000000 ) ) ;
#6748 = CARTESIAN_POINT ( 'NONE',  ( 205.0000000000000284, 8.660254037844390851, 145.0000000000000284 ) ) ;
#6749 = DIRECTION ( 'NONE',  ( 1.000000000000000000, 0.000000000000000000, 0.000000000000000000 ) ) ;
#6750 = EDGE_CURVE ( 'NONE', #918, #5766, #5686, .T. ) ;
#6751 = VERTEX_POINT ( 'NONE', #3276 ) ;
#6752 = CARTESIAN_POINT ( 'NONE',  ( 395.0000000000000000, 8.660254037844390851, 140.0000000000000000 ) ) ;
#6753 = AXIS2_PLACEMENT_3D ( 'NONE', #5432, #7054, #4165 ) ;
#6754 = VECTOR ( 'NONE', #1120, 1000.000000000000000 ) ;
#6755 = VERTEX_POINT ( 'NONE', #601 ) ;
#6756 = EDGE_LOOP ( 'NONE', ( #592, #284 ) ) ;
#6757 = CARTESIAN_POINT ( 'NONE',  ( -13.50000000000000000, 0.000000000000000000, -121.0000000000000000 ) ) ;
#6758 = CARTESIAN_POINT ( 'NONE',  ( -0.1410422978106123659, 4.700232962125094893, -3.687027686973624707 ) ) ;
#6759 = LINE ( 'NONE', #4427, #4804 ) ;
#6760 = CARTESIAN_POINT ( 'NONE',  ( 155.0000000000000000, 8.660254037844390851, 145.0000000000000284 ) ) ;
#6761 = VECTOR ( 'NONE', #2136, 1000.000000000000000 ) ;
#6762 = CARTESIAN_POINT ( 'NONE',  ( 386.6666666666666288, -20.00000000000000000, -162.5000000000000853 ) ) ;
#6763 = UNCERTAINTY_MEASURE_WITH_UNIT (LENGTH_MEASURE( 1.000000000000000082E-05 ), #6290, 'distance_accuracy_value', 'NONE');
#6764 = B_SPLINE_CURVE_WITH_KNOTS ( 'NONE', 3,
 ( #42, #6331, #705, #1225, #5231, #3710, #5760, #6401 ),
 .UNSPECIFIED., .F., .F.,
 ( 4, 2, 2, 4 ),
 ( 2.465131517071352357E-07, 0.001183067374689843057, 0.001774477805458910071, 0.002365888236227977302 ),
 .UNSPECIFIED. ) ;
#6765 = CARTESIAN_POINT ( 'NONE',  ( 114.9999999999999858, 8.660254037844390851, 140.0000000000000000 ) ) ;
#6766 =( REPRESENTATION_RELATIONSHIP ('NONE','NONE', #5587, #951 ) REPRESENTATION_RELATIONSHIP_WITH_TRANSFORMATION ( #282 )SHAPE_REPRESENTATION_RELATIONSHIP( ) );
#6767 = EDGE_LOOP ( 'NONE', ( #749, #1745, #6886, #6099 ) ) ;
#6768 = MECHANICAL_DESIGN_GEOMETRIC_PRESENTATION_REPRESENTATION (  '', ( #2795 ), #5309 ) ;
#6769 = CARTESIAN_POINT ( 'NONE',  ( 445.0000000000000000, -8.660254037844389075, 139.9990000000000236 ) ) ;
#6770 = LINE ( 'NONE', #2176, #559 ) ;
#6771 = FACE_BOUND ( 'NONE', #943, .T. ) ;
#6772 = PLANE ( 'NONE',  #254 ) ;
#6773 = AXIS2_PLACEMENT_3D ( 'NONE', #297, #1960, #6667 ) ;
#6774 = DIRECTION ( 'NONE',  ( -0.000000000000000000, 1.000000000000000000, 0.000000000000000000 ) ) ;
#6775 = ORIENTED_EDGE ( 'NONE', *, *, #3341, .F. ) ;
#6776 = ORIENTED_EDGE ( 'NONE', *, *, #3401, .F. ) ;
#6777 = EDGE_CURVE ( 'NONE', #2492, #563, #6642, .T. ) ;
#6778 = AXIS2_PLACEMENT_3D ( 'NONE', #1671, #2229, #3961 ) ;
#6779 = ORIENTED_EDGE ( 'NONE', *, *, #1153, .F. ) ;
#6780 = AXIS2_PLACEMENT_3D ( 'NONE', #2876, #63, #1793 ) ;
#6781 = LINE ( 'NONE', #4527, #1623 ) ;
#6782 = CARTESIAN_POINT ( 'NONE',  ( 303.3333333333333144, -20.00000000000000000, -162.5000000000000853 ) ) ;
#6783 = CIRCLE ( 'NONE', #6658, 13.50000000000000000 ) ;
#6784 = ORIENTED_EDGE ( 'NONE', *, *, #5085, .F. ) ;
#6785 = DIRECTION ( 'NONE',  ( -0.000000000000000000, 1.000000000000000000, -0.000000000000000000 ) ) ;
#6786 = ADVANCED_FACE ( 'NONE', ( #1609 ), #2806, .T. ) ;
#6787 = DIRECTION ( 'NONE',  ( 0.000000000000000000, 0.000000000000000000, 1.000000000000000000 ) ) ;
#6788 = CARTESIAN_POINT ( 'NONE',  ( 19.00000000000000000, 2.326828918379970970E-15, 125.0000000000000000 ) ) ;
#6789 = EDGE_CURVE ( 'NONE', #6755, #1207, #1087, .T. ) ;
#6790 = AXIS2_PLACEMENT_3D ( 'NONE', #7071, #152, #5234 ) ;
#6791 = DIRECTION ( 'NONE',  ( 6.123233995736766036E-17, -1.000000000000000000, 0.000000000000000000 ) ) ;
#6792 = ORIENTED_EDGE ( 'NONE', *, *, #3141, .T. ) ;
#6793 = CARTESIAN_POINT ( 'NONE',  ( 114.9999999999999858, 8.660254037844390851, 145.0000000000000284 ) ) ;
#6794 = ORIENTED_EDGE ( 'NONE', *, *, #1002, .F. ) ;
#6795 = ORIENTED_EDGE ( 'NONE', *, *, #3843, .T. ) ;
#6796 = EDGE_CURVE ( 'NONE', #310, #1933, #2265, .T. ) ;
#6797 = DIRECTION ( 'NONE',  ( -0.000000000000000000, -0.000000000000000000, -1.000000000000000000 ) ) ;
#6798 = DIRECTION ( 'NONE',  ( 0.000000000000000000, 0.000000000000000000, -1.000000000000000000 ) ) ;
#6799 = ITEM_DEFINED_TRANSFORMATION ( 'NONE', 'NONE', #6400,  #1963 ) ;
#6800 = DIRECTION ( 'NONE',  ( 0.000000000000000000, -0.000000000000000000, 1.000000000000000000 ) ) ;
#6801 = PLANE ( 'NONE',  #4877 ) ;
#6802 = CIRCLE ( 'NONE', #98, 4.250000000000000000 ) ;
#6803 = ORIENTED_EDGE ( 'NONE', *, *, #2980, .T. ) ;
#6804 = DIRECTION ( 'NONE',  ( -0.000000000000000000, -0.000000000000000000, -1.000000000000000000 ) ) ;
#6805 = ORIENTED_EDGE ( 'NONE', *, *, #3316, .F. ) ;
#6806 = PLANE ( 'NONE',  #2390 ) ;
#6807 = CARTESIAN_POINT ( 'NONE',  ( 395.0000000000000000, 8.660254037844390851, 145.0000000000000284 ) ) ;
#6808 = CARTESIAN_POINT ( 'NONE',  ( -20.63749999999999929, 1.224646799147352862E-15, 9.999999999999996447 ) ) ;
#6809 = DIRECTION ( 'NONE',  ( -0.000000000000000000, 0.000000000000000000, -1.000000000000000000 ) ) ;
#6810 = B_SPLINE_CURVE_WITH_KNOTS ( 'NONE', 3,
 ( #7272, #5459, #4942, #978, #4863 ),
 .UNSPECIFIED., .F., .F.,
 ( 4, 1, 4 ),
 ( 5.640274452250024914E-20, 0.002309401076758505356, 0.004618802153517010713 ),
 .UNSPECIFIED. ) ;
#6811 = DIRECTION ( 'NONE',  ( 0.000000000000000000, 0.4999999999999993894, -0.8660254037844389297 ) ) ;
#6812 = VERTEX_POINT ( 'NONE', #6788 ) ;
#6813 = AXIS2_PLACEMENT_3D ( 'NONE', #5992, #425, #2687 ) ;
#6814 = VERTEX_POINT ( 'NONE', #3893 ) ;
#6815 = CARTESIAN_POINT ( 'NONE',  ( 240.0000000000000000, 0.000000000000000000, -123.0000000000000000 ) ) ;
#6816 = VERTEX_POINT ( 'NONE', #3353 ) ;
#6817 = CARTESIAN_POINT ( 'NONE',  ( 435.0000000000000568, -8.660254037844389075, 140.0000000000000000 ) ) ;
#6818 = EDGE_CURVE ( 'NONE', #1413, #266, #44, .T. ) ;
#6819 = CARTESIAN_POINT ( 'NONE',  ( 219.9999999999999716, -14.99999999999999822, 162.5000000000000853 ) ) ;
#6820 = EDGE_LOOP ( 'NONE', ( #204, #6698 ) ) ;
#6821 = CARTESIAN_POINT ( 'NONE',  ( 4.000000000000000000, 0.000000000000000000, 0.000000000000000000 ) ) ;
#6822 = DIRECTION ( 'NONE',  ( 0.000000000000000000, 0.000000000000000000, -1.000000000000000000 ) ) ;
#6823 = FACE_OUTER_BOUND ( 'NONE', #5270, .T. ) ;
#6824 = DIRECTION ( 'NONE',  ( 0.000000000000000000, 0.000000000000000000, 1.000000000000000000 ) ) ;
#6825 = EDGE_CURVE ( 'NONE', #3661, #3696, #1124, .T. ) ;
#6826 = EDGE_LOOP ( 'NONE', ( #2703, #6738, #3355, #6794 ) ) ;
#6827 = CARTESIAN_POINT ( 'NONE',  ( 355.0000000000000000, -8.660254037844389075, 145.0000000000000284 ) ) ;
#6828 = EDGE_CURVE ( 'NONE', #2887, #5784, #5579, .T. ) ;
#6829 = ORIENTED_EDGE ( 'NONE', *, *, #1406, .F. ) ;
#6830 = CYLINDRICAL_SURFACE ( 'NONE', #369, 2.100000000000000089 ) ;
#6831 = CARTESIAN_POINT ( 'NONE',  ( 470.0000000000000000, -20.00000000000000000, 140.0000000000000000 ) ) ;
#6832 = CONTEXT_DEPENDENT_SHAPE_REPRESENTATION ( #2517, #3730 ) ;
#6833 = CARTESIAN_POINT ( 'NONE',  ( 0.000000000000000000, 0.000000000000000000, -121.0000000000000000 ) ) ;
#6834 = CARTESIAN_POINT ( 'NONE',  ( 0.000000000000000000, 0.000000000000000000, -125.0000000000000000 ) ) ;
#6835 = EDGE_LOOP ( 'NONE', ( #3, #7077, #3883 ) ) ;
#6836 = DIRECTION ( 'NONE',  ( -0.000000000000000000, -0.000000000000000000, -1.000000000000000000 ) ) ;
#6837 = EDGE_CURVE ( 'NONE', #6108, #5618, #5160, .T. ) ;
#6838 = ORIENTED_EDGE ( 'NONE', *, *, #1444, .T. ) ;
#6839 = DIRECTION ( 'NONE',  ( -0.000000000000000000, -0.000000000000000000, 1.000000000000000000 ) ) ;
#6840 = DIRECTION ( 'NONE',  ( 0.000000000000000000, 1.000000000000000000, 0.000000000000000000 ) ) ;
#6841 = CARTESIAN_POINT ( 'NONE',  ( 303.3333333333333144, -15.00000000000000000, 162.5000000000000853 ) ) ;
#6842 = CARTESIAN_POINT ( 'NONE',  ( 53.33333333333330017, -14.99999999999999822, 162.5000000000000853 ) ) ;
#6843 = CONICAL_SURFACE ( 'NONE', #3579, 2.055000000000000160, 0.7853981633974721488 ) ;
#6844=STYLED_ITEM('',(#7446),#5831);
#6845 = LINE ( 'NONE', #2916, #3865 ) ;
#6846 = EDGE_CURVE ( 'NONE', #2062, #3817, #3430, .T. ) ;
#6847 = VERTEX_POINT ( 'NONE', #2856 ) ;
#6848 = SHAPE_DEFINITION_REPRESENTATION ( #1342, #1193 ) ;
#6849 = ORIENTED_EDGE ( 'NONE', *, *, #1435, .F. ) ;
#6850 = CARTESIAN_POINT ( 'NONE',  ( -2.000000000000001776, 0.000000000000000000, 0.000000000000000000 ) ) ;
#6851 = EDGE_CURVE ( 'NONE', #4048, #4599, #3318, .T. ) ;
#6852 = VECTOR ( 'NONE', #1174, 1000.000000000000000 ) ;
#6853 = LINE ( 'NONE', #2825, #2445 ) ;
#6854 = EDGE_LOOP ( 'NONE', ( #1958, #2042, #810, #7047 ) ) ;
#6855 = CIRCLE ( 'NONE', #5773, 0.2000000000000022593 ) ;
#6856 = DIRECTION ( 'NONE',  ( 0.000000000000000000, 1.000000000000000000, 0.000000000000000000 ) ) ;
#6857 = CARTESIAN_POINT ( 'NONE',  ( 470.0000000000000000, -20.00000000000000000, 180.0000000000000284 ) ) ;
#6858 = DIRECTION ( 'NONE',  ( 1.000000000000000000, 0.000000000000000000, 0.000000000000000000 ) ) ;
#6859 = ORIENTED_EDGE ( 'NONE', *, *, #5485, .T. ) ;
#6860 = CARTESIAN_POINT ( 'NONE',  ( 0.000000000000000000, 0.000000000000000000, -4.694516984716113228 ) ) ;
#6861 = CONICAL_SURFACE ( 'NONE', #3606, 4.000000000000000000, 0.8911886515913786111 ) ;
#6862 = EDGE_CURVE ( 'NONE', #1770, #7340, #5927, .T. ) ;
#6863 = ORIENTED_EDGE ( 'NONE', *, *, #948, .T. ) ;
#6864 = CARTESIAN_POINT ( 'NONE',  ( 386.6666666666666288, -20.00000000000000000, 162.5000000000000853 ) ) ;
#6865 = CYLINDRICAL_SURFACE ( 'NONE', #5575, 2.649999999999985700 ) ;
#6866 = FACE_OUTER_BOUND ( 'NONE', #7212, .T. ) ;
#6867 = DIRECTION ( 'NONE',  ( -0.000000000000000000, -0.000000000000000000, 1.000000000000000000 ) ) ;
#6868 = PRESENTATION_LAYER_ASSIGNMENT (  '', '', ( #3378 ) ) ;
#6869 = EDGE_LOOP ( 'NONE', ( #5186, #3472, #4288, #3789 ) ) ;
#6870 = AXIS2_PLACEMENT_3D ( 'NONE', #5049, #2673, #489 ) ;
#6871 = CARTESIAN_POINT ( 'NONE',  ( -2.000000000000001776, 0.000000000000000000, 0.000000000000000000 ) ) ;
#6872 = AXIS2_PLACEMENT_3D ( 'NONE', #7162, #2615, #3128 ) ;
#6873 = CIRCLE ( 'NONE', #4609, 0.2000000000000022593 ) ;
#6874 = B_SPLINE_CURVE_WITH_KNOTS ( 'NONE', 3,
 ( #3148, #5983, #5525, #4329, #5450 ),
 .UNSPECIFIED., .F., .F.,
 ( 4, 1, 4 ),
 ( 0.000000000000000000, 0.002309401076758506657, 0.004618802153517013315 ),
 .UNSPECIFIED. ) ;
#6875 = VERTEX_POINT ( 'NONE', #6302 ) ;
#6876 = CARTESIAN_POINT ( 'NONE',  ( 0.7826237921249277196, 0.000000000000000000, 0.000000000000000000 ) ) ;
#6877 = DIRECTION ( 'NONE',  ( 1.000000000000000000, 0.000000000000000000, 0.000000000000000000 ) ) ;
#6878 = EDGE_CURVE ( 'NONE', #2674, #3068, #311, .T. ) ;
#6879 = DIRECTION ( 'NONE',  ( -0.000000000000000000, 1.000000000000000000, -0.000000000000000000 ) ) ;
#6880 = LINE ( 'NONE', #1767, #7229 ) ;
#6881 = VECTOR ( 'NONE', #7012, 1000.000000000000000 ) ;
#6882 = EDGE_CURVE ( 'NONE', #1976, #431, #2197, .T. ) ;
#6883 = EDGE_CURVE ( 'NONE', #3397, #3428, #6897, .T. ) ;
#6884 = CARTESIAN_POINT ( 'NONE',  ( 155.0000000000000000, -8.660254037844389075, 140.0000000000000000 ) ) ;
#6885 = AXIS2_PLACEMENT_3D ( 'NONE', #353, #4350, #2734 ) ;
#6886 = ORIENTED_EDGE ( 'NONE', *, *, #7013, .T. ) ;
#6887 = ORIENTED_EDGE ( 'NONE', *, *, #849, .T. ) ;
#6888 = APPLICATION_PROTOCOL_DEFINITION ( 'draft international standard', 'automotive_design', 1998, #3620 ) ;
#6889 = ORIENTED_EDGE ( 'NONE', *, *, #727, .F. ) ;
#6890 = EDGE_CURVE ( 'NONE', #3280, #4492, #5022, .T. ) ;
#6891 = VECTOR ( 'NONE', #2313, 1000.000000000000000 ) ;
#6892 = DIRECTION ( 'NONE',  ( 0.000000000000000000, 1.000000000000000000, 0.000000000000000000 ) ) ;
#6893 = CIRCLE ( 'NONE', #898, 2.649999999999985700 ) ;
#6894 = VERTEX_POINT ( 'NONE', #1994 ) ;
#6895 = CIRCLE ( 'NONE', #1741, 19.00000000000000000 ) ;
#6896 = DIRECTION ( 'NONE',  ( 0.000000000000000000, 0.000000000000000000, 1.000000000000000000 ) ) ;
#6897 = LINE ( 'NONE', #1646, #3405 ) ;
#6898 = CIRCLE ( 'NONE', #447, 11.00000000000000000 ) ;
#6899 = ORIENTED_EDGE ( 'NONE', *, *, #2281, .T. ) ;
#6900 = PRODUCT_DEFINITION_SHAPE ( 'NONE', 'NONE',  #7391 ) ;
#6901 = CARTESIAN_POINT ( 'NONE',  ( -5.000000000000000888, 8.660254037844390851, 150.0000000000000000 ) ) ;
#6902 = ORIENTED_EDGE ( 'NONE', *, *, #1414, .T. ) ;
#6903 = FACE_OUTER_BOUND ( 'NONE', #4884, .T. ) ;
#6904 = CIRCLE ( 'NONE', #3780, 2.649999999999985700 ) ;
#6905 = DIRECTION ( 'NONE',  ( 0.000000000000000000, 0.000000000000000000, -1.000000000000000000 ) ) ;
#6906 = CONTEXT_DEPENDENT_SHAPE_REPRESENTATION ( #1388, #4740 ) ;
#6907 = CARTESIAN_POINT ( 'NONE',  ( 395.0000000000000000, -8.660254037844389075, 140.0000000000000000 ) ) ;
#6908 = CARTESIAN_POINT ( 'NONE',  ( 4.999999999999999112, -8.660254037844389075, 150.0000000000000000 ) ) ;
#6909 =( REPRESENTATION_RELATIONSHIP ('NONE','NONE', #5587, #5023 ) REPRESENTATION_RELATIONSHIP_WITH_TRANSFORMATION ( #3061 )SHAPE_REPRESENTATION_RELATIONSHIP( ) );
#6910 = ORIENTED_EDGE ( 'NONE', *, *, #2815, .F. ) ;
#6911 = CARTESIAN_POINT ( 'NONE',  ( 4.197393957002303999, -0.4069871074557456780, -3.503767560748925813 ) ) ;
#6912 = EDGE_CURVE ( 'NONE', #431, #1288, #1149, .T. ) ;
#6913 = EDGE_LOOP ( 'NONE', ( #5801, #4227, #6185, #6607 ) ) ;
#6914 = PLANE ( 'NONE',  #2625 ) ;
#6915 = CARTESIAN_POINT ( 'NONE',  ( -1.257172072275743346, 3.892973519171203378, -3.433252694550776862 ) ) ;
#6916 = DIRECTION ( 'NONE',  ( 0.000000000000000000, 1.000000000000000000, 0.000000000000000000 ) ) ;
#6917 = LINE ( 'NONE', #5120, #4811 ) ;
#6918 = ADVANCED_FACE ( 'NONE', ( #6823 ), #1678, .F. ) ;
#6919 = ORIENTED_EDGE ( 'NONE', *, *, #1613, .F. ) ;
#6920 = DIRECTION ( 'NONE',  ( 0.000000000000000000, 0.000000000000000000, 1.000000000000000000 ) ) ;
#6921 = EDGE_LOOP ( 'NONE', ( #25, #4410, #2863, #6244 ) ) ;
#6922 = LINE ( 'NONE', #4060, #6190 ) ;
#6923 = EDGE_CURVE ( 'NONE', #5777, #3673, #4637, .T. ) ;
#6924 = EDGE_LOOP ( 'NONE', ( #4960, #1709 ) ) ;
#6925 = FILL_AREA_STYLE_COLOUR ( '', #4265 ) ;
#6926 = EDGE_CURVE ( 'NONE', #2205, #1598, #4064, .T. ) ;
#6927 = DIRECTION ( 'NONE',  ( -0.000000000000000000, 1.000000000000000000, -0.000000000000000000 ) ) ;
#6928 = ORIENTED_EDGE ( 'NONE', *, *, #4174, .F. ) ;
#6929 = CARTESIAN_POINT ( 'NONE',  ( -0.2277608394786177770, 0.000000000000000000, 0.000000000000000000 ) ) ;
#6930 = EDGE_LOOP ( 'NONE', ( #4523, #7171, #6350, #750 ) ) ;
#6931 = ORIENTED_EDGE ( 'NONE', *, *, #2234, .F. ) ;
#6932 = PLANE ( 'NONE',  #5076 ) ;
#6933 = CARTESIAN_POINT ( 'NONE',  ( -30.00000000000002842, -20.00000000000000000, 140.0000000000000000 ) ) ;
#6934 = CYLINDRICAL_SURFACE ( 'NONE', #3758, 2.500000000000000888 ) ;
#6935 = ORIENTED_EDGE ( 'NONE', *, *, #6657, .F. ) ;
#6936 = DIRECTION ( 'NONE',  ( 0.000000000000000000, 0.000000000000000000, 1.000000000000000000 ) ) ;
#6937 = EDGE_LOOP ( 'NONE', ( #5177, #5856 ) ) ;
#6938 = CARTESIAN_POINT ( 'NONE',  ( 75.00000000000001421, 8.660254037844390851, 145.0000000000000284 ) ) ;
#6939 = CARTESIAN_POINT ( 'NONE',  ( -4.141042297810615835, 2.227970268150415656, -3.687027686973619822 ) ) ;
#6940 = CARTESIAN_POINT ( 'NONE',  ( -5.000000000000000888, -8.660254037844389075, 140.0000000000000000 ) ) ;
#6941 = FACE_BOUND ( 'NONE', #4081, .T. ) ;
#6942 = DIRECTION ( 'NONE',  ( 0.000000000000000000, 0.000000000000000000, 1.000000000000000000 ) ) ;
#6943 = ORIENTED_EDGE ( 'NONE', *, *, #6376, .F. ) ;
#6944 = ORIENTED_EDGE ( 'NONE', *, *, #4247, .F. ) ;
#6945 = VECTOR ( 'NONE', #5217, 1000.000000000000000 ) ;
#6946 = CARTESIAN_POINT ( 'NONE',  ( 219.9999999999999716, -20.00000000000000000, 159.8500000000001080 ) ) ;
#6947 = EDGE_LOOP ( 'NONE', ( #3134, #2812, #5308, #5907 ) ) ;
#6948 = EDGE_CURVE ( 'NONE', #1142, #3854, #2088, .T. ) ;
#6949 = PRODUCT_DEFINITION_SHAPE ( 'NONE', 'NONE',  #7379 ) ;
#6950 = SURFACE_STYLE_FILL_AREA ( #6989 ) ;
#6951 = VECTOR ( 'NONE', #6527, 1000.000000000000000 ) ;
#6952 = DIRECTION ( 'NONE',  ( 1.000000000000000000, 0.000000000000000000, 0.000000000000000000 ) ) ;
#6953 = ORIENTED_EDGE ( 'NONE', *, *, #3120, .F. ) ;
#6954 = PRESENTATION_STYLE_ASSIGNMENT (( #4665 ) ) ;
#6955 = LINE ( 'NONE', #2402, #2911 ) ;
#6956 = EDGE_CURVE ( 'NONE', #818, #6064, #737, .T. ) ;
#6957 = ORIENTED_EDGE ( 'NONE', *, *, #5251, .F. ) ;
#6958 = SURFACE_SIDE_STYLE ('',( #781 ) ) ;
#6959 = VERTEX_POINT ( 'NONE', #5303 ) ;
#6960 = AXIS2_PLACEMENT_3D ( 'NONE', #2039, #6034, #4334 ) ;
#6961 = AXIS2_PLACEMENT_3D ( 'NONE', #633, #5400, #2400 ) ;
#6962 = FACE_OUTER_BOUND ( 'NONE', #6826, .T. ) ;
#6963 = CARTESIAN_POINT ( 'NONE',  ( 0.000000000000000000, 0.000000000000000000, -5.000000000000000888 ) ) ;
#6964 = ITEM_DEFINED_TRANSFORMATION ( 'NONE', 'NONE', #2663,  #1963 ) ;
#6965 = LINE ( 'NONE', #5875, #738 ) ;
#6966 = CARTESIAN_POINT ( 'NONE',  ( 386.6666666666666288, -15.00000000000000000, 162.5000000000000853 ) ) ;
#6967 = EDGE_CURVE ( 'NONE', #5784, #2308, #6402, .T. ) ;
#6968 = ORIENTED_EDGE ( 'NONE', *, *, #1510, .F. ) ;
#6969 = CARTESIAN_POINT ( 'NONE',  ( 2.500000000000000000, 1.178949249685218525, 2.041999999999999371 ) ) ;
#6970 = PRODUCT_DEFINITION_SHAPE ( 'NONE', 'NONE',  #7368 ) ;
#6971 = VERTEX_POINT ( 'NONE', #1810 ) ;
#6972 = ORIENTED_EDGE ( 'NONE', *, *, #4602, .T. ) ;
#6973 = FACE_OUTER_BOUND ( 'NONE', #307, .T. ) ;
#6974 = DIRECTION ( 'NONE',  ( -1.000000000000000000, -0.000000000000000000, -0.000000000000000000 ) ) ;
#6975 = DIRECTION ( 'NONE',  ( 1.000000000000000000, 0.000000000000000000, 0.000000000000000000 ) ) ;
#6976 = CARTESIAN_POINT ( 'NONE',  ( 2.500000000000000000, -1.178949249685213863, 2.042000000000002924 ) ) ;
#6977 = AXIS2_PLACEMENT_3D ( 'NONE', #4236, #6532, #726 ) ;
#6978 = AXIS2_PLACEMENT_3D ( 'NONE', #379, #4940, #6112 ) ;
#6979 = CIRCLE ( 'NONE', #3733, 4.250000000000000000 ) ;
#6980 = CARTESIAN_POINT ( 'NONE',  ( 0.000000000000000000, -8.660254037844389075, 140.0000000000000000 ) ) ;
#6981 = VECTOR ( 'NONE', #1532, 1000.000000000000000 ) ;
#6982 = AXIS2_PLACEMENT_3D ( 'NONE', #32, #4521, #6811 ) ;
#6983 = ORIENTED_EDGE ( 'NONE', *, *, #43, .F. ) ;
#6984 = AXIS2_PLACEMENT_3D ( 'NONE', #2499, #243, #912 ) ;
#6985 = VECTOR ( 'NONE', #2280, 1000.000000000000000 ) ;
#6986 = CONTEXT_DEPENDENT_SHAPE_REPRESENTATION ( #6611, #2525 ) ;
#6987 = CARTESIAN_POINT ( 'NONE',  ( 303.3333333333333144, -25.00000000000000000, 162.5000000000000853 ) ) ;
#6988 = VERTEX_POINT ( 'NONE', #777 ) ;
#6989 = FILL_AREA_STYLE ('',( #2363 ) ) ;
#6990 = CIRCLE ( 'NONE', #770, 10.72499999999999964 ) ;
#6991 = DIRECTION ( 'NONE',  ( -1.000000000000000000, 0.000000000000000000, 0.000000000000000000 ) ) ;
#6992 = EDGE_CURVE ( 'NONE', #3333, #1043, #7114, .T. ) ;
#6993 = ORIENTED_EDGE ( 'NONE', *, *, #2003, .T. ) ;
#6994 =( REPRESENTATION_RELATIONSHIP ('NONE','NONE', #5587, #5023 ) REPRESENTATION_RELATIONSHIP_WITH_TRANSFORMATION ( #4613 )SHAPE_REPRESENTATION_RELATIONSHIP( ) );
#6995 = AXIS2_PLACEMENT_3D ( 'NONE', #6966, #3657, #2936 ) ;
#6996 = AXIS2_PLACEMENT_3D ( 'NONE', #2238, #4324, #2150 ) ;
#6997 = DIRECTION ( 'NONE',  ( 0.000000000000000000, 0.000000000000000000, -1.000000000000000000 ) ) ;
#6998 = LINE ( 'NONE', #1851, #6174 ) ;
#6999 = DIRECTION ( 'NONE',  ( 0.000000000000000000, 1.000000000000000000, 0.000000000000000000 ) ) ;
#7000 = CIRCLE ( 'NONE', #73, 2.499999999999999556 ) ;
#7001 = CARTESIAN_POINT ( 'NONE',  ( -31.74999999999995737, 5.204748896376250699E-16, -4.250000000000000000 ) ) ;
#7002 = AXIS2_PLACEMENT_3D ( 'NONE', #27, #2426, #1765 ) ;
#7003 = ORIENTED_EDGE ( 'NONE', *, *, #6581, .T. ) ;
#7004 = EDGE_CURVE ( 'NONE', #2874, #3280, #2369, .T. ) ;
#7005 = EDGE_CURVE ( 'NONE', #3802, #6894, #634, .T. ) ;
#7006 = CYLINDRICAL_SURFACE ( 'NONE', #6709, 2.500000000000000888 ) ;
#7007 = DIRECTION ( 'NONE',  ( -0.000000000000000000, -1.000000000000000000, -0.000000000000000000 ) ) ;
#7008 = CONTEXT_DEPENDENT_SHAPE_REPRESENTATION ( #497, #5870 ) ;
#7009 = CARTESIAN_POINT ( 'NONE',  ( 1.360585162435110629, -4.061296242128317857, -3.505054077164905024 ) ) ;
#7010 = CARTESIAN_POINT ( 'NONE',  ( -30.00000000000002842, -25.00000000000000000, 200.0000000000000000 ) ) ;
#7011 = ORIENTED_EDGE ( 'NONE', *, *, #2190, .T. ) ;
#7012 = DIRECTION ( 'NONE',  ( 0.000000000000000000, -1.000000000000000000, 0.000000000000000000 ) ) ;
#7013 = EDGE_CURVE ( 'NONE', #4390, #7221, #7000, .T. ) ;
#7014 = ORIENTED_EDGE ( 'NONE', *, *, #113, .F. ) ;
#7015 = VECTOR ( 'NONE', #4598, 1000.000000000000000 ) ;
#7016 = VERTEX_POINT ( 'NONE', #5232 ) ;
#7017 = CARTESIAN_POINT ( 'NONE',  ( 0.000000000000000000, 2.357898499370433054, -1.951563910473907981E-15 ) ) ;
#7018 = CARTESIAN_POINT ( 'NONE',  ( -4.175648173966055587, 2.207990556236529844, -3.469390959564062626 ) ) ;
#7019 = CARTESIAN_POINT ( 'NONE',  ( -2.059999999999998721, 2.522772406243545965E-16, -0.3080913168122742518 ) ) ;
#7020 = DIRECTION ( 'NONE',  ( -0.000000000000000000, -0.000000000000000000, 1.000000000000000000 ) ) ;
#7021 = VECTOR ( 'NONE', #5, 1000.000000000000000 ) ;
#7022 = CARTESIAN_POINT ( 'NONE',  ( 4.999999999999999112, -8.660254037844389075, 150.0000000000000000 ) ) ;
#7023 = ORIENTED_EDGE ( 'NONE', *, *, #6828, .T. ) ;
#7024 = ORIENTED_EDGE ( 'NONE', *, *, #3601, .T. ) ;
#7025 = ITEM_DEFINED_TRANSFORMATION ( 'NONE', 'NONE', #4366,  #1963 ) ;
#7026 = FACE_OUTER_BOUND ( 'NONE', #6258, .T. ) ;
#7027 = VERTEX_POINT ( 'NONE', #7067 ) ;
#7028 = EDGE_CURVE ( 'NONE', #2892, #2821, #1029, .T. ) ;
#7029 = FACE_OUTER_BOUND ( 'NONE', #798, .T. ) ;
#7030 = EDGE_LOOP ( 'NONE', ( #5122, #161, #6779, #7065 ) ) ;
#7031 = EDGE_CURVE ( 'NONE', #3206, #2826, #6955, .T. ) ;
#7032 = DIRECTION ( 'NONE',  ( 0.000000000000000000, 0.000000000000000000, -1.000000000000000000 ) ) ;
#7033 = CARTESIAN_POINT ( 'NONE',  ( 2.500000000000000000, 0.000000000000000000, 0.000000000000000000 ) ) ;
#7034 = DIRECTION ( 'NONE',  ( 0.000000000000000000, 0.000000000000000000, 1.000000000000000000 ) ) ;
#7035 =( REPRESENTATION_RELATIONSHIP ('NONE','NONE', #5587, #1193 ) REPRESENTATION_RELATIONSHIP_WITH_TRANSFORMATION ( #195 )SHAPE_REPRESENTATION_RELATIONSHIP( ) );
#7036 = ORIENTED_EDGE ( 'NONE', *, *, #5038, .T. ) ;
#7037 = DIRECTION ( 'NONE',  ( -0.000000000000000000, 1.000000000000000000, -0.000000000000000000 ) ) ;
#7038 = EDGE_CURVE ( 'NONE', #2383, #1770, #5196, .T. ) ;
#7039 = CONTEXT_DEPENDENT_SHAPE_REPRESENTATION ( #3295, #6306 ) ;
#7040 = CARTESIAN_POINT ( 'NONE',  ( -0.02448733951239248641, -4.877042772274742255, -3.751161874094027571 ) ) ;
#7041 = FACE_OUTER_BOUND ( 'NONE', #6582, .T. ) ;
#7042 = CARTESIAN_POINT ( 'NONE',  ( 0.000000000000000000, 0.000000000000000000, 0.000000000000000000 ) ) ;
#7043 = ADVANCED_FACE ( 'NONE', ( #5340 ), #6362, .F. ) ;
#7044 = ORIENTED_EDGE ( 'NONE', *, *, #6878, .T. ) ;
#7045 = CARTESIAN_POINT ( 'NONE',  ( 136.6666666666666288, -15.00000000000000000, 165.1500000000000625 ) ) ;
#7046 = VERTEX_POINT ( 'NONE', #1196 ) ;
#7047 = ORIENTED_EDGE ( 'NONE', *, *, #2980, .F. ) ;
#7048 = DIRECTION ( 'NONE',  ( -1.000000000000000000, -0.000000000000000000, -0.000000000000000000 ) ) ;
#7049 = CARTESIAN_POINT ( 'NONE',  ( -4.175002511812151873, -2.208363329454905877, -3.469254087858246738 ) ) ;
#7050 = CARTESIAN_POINT ( 'NONE',  ( 53.33333333333330017, -20.00000000000000000, 162.5000000000000853 ) ) ;
#7051 = LINE ( 'NONE', #6453, #180 ) ;
#7052 = EDGE_CURVE ( 'NONE', #4934, #3114, #6471, .T. ) ;
#7053 = CARTESIAN_POINT ( 'NONE',  ( 386.6666666666666288, -25.00000000000000000, 162.5000000000000853 ) ) ;
#7054 = DIRECTION ( 'NONE',  ( -0.000000000000000000, -0.000000000000000000, 1.000000000000000000 ) ) ;
#7055 = ORIENTED_EDGE ( 'NONE', *, *, #1414, .F. ) ;
#7056 = ITEM_DEFINED_TRANSFORMATION ( 'NONE', 'NONE', #3022,  #1963 ) ;
#7057 = CYLINDRICAL_SURFACE ( 'NONE', #6155, 4.250000000000000000 ) ;
#7058 = ORIENTED_EDGE ( 'NONE', *, *, #3499, .F. ) ;
#7059 = AXIS2_PLACEMENT_3D ( 'NONE', #1231, #4147, #1202 ) ;
#7060 = EDGE_CURVE ( 'NONE', #763, #1652, #5836, .T. ) ;
#7061 = CARTESIAN_POINT ( 'NONE',  ( 0.000000000000000000, 0.000000000000000000, -5.000000000000000000 ) ) ;
#7062 = UNCERTAINTY_MEASURE_WITH_UNIT (LENGTH_MEASURE( 1.000000000000000082E-05 ), #4138, 'distance_accuracy_value', 'NONE');
#7063 = CIRCLE ( 'NONE', #3831, 4.000000000000000000 ) ;
#7064 = ORIENTED_EDGE ( 'NONE', *, *, #5313, .T. ) ;
#7065 = ORIENTED_EDGE ( 'NONE', *, *, #2955, .F. ) ;
#7066 = LINE ( 'NONE', #4475, #4440 ) ;
#7067 = CARTESIAN_POINT ( 'NONE',  ( 4.999999999999999112, 8.660254037844390851, 145.0000000000000284 ) ) ;
#7068 = AXIS2_PLACEMENT_3D ( 'NONE', #3207, #2704, #6653 ) ;
#7069 = ORIENTED_EDGE ( 'NONE', *, *, #3778, .T. ) ;
#7070 = PRODUCT_DEFINITION_SHAPE ( 'NONE', 'NONE',  #7400 ) ;
#7071 = CARTESIAN_POINT ( 'NONE',  ( 35.00000000000000000, 8.660254037844390851, 139.9990000000000236 ) ) ;
#7072 = ORIENTED_EDGE ( 'NONE', *, *, #3853, .T. ) ;
#7073 = CARTESIAN_POINT ( 'NONE',  ( 4.204115023516791005, -1.660442669500199919, -3.602151381774560068 ) ) ;
#7074 = CONTEXT_DEPENDENT_SHAPE_REPRESENTATION ( #4304, #5752 ) ;
#7075 = DIRECTION ( 'NONE',  ( -1.000000000000000000, -0.000000000000000000, -0.000000000000000000 ) ) ;
#7076 = DIRECTION ( 'NONE',  ( 0.000000000000000000, 0.000000000000000000, 1.000000000000000000 ) ) ;
#7077 = ORIENTED_EDGE ( 'NONE', *, *, #1653, .F. ) ;
#7078 = FACE_OUTER_BOUND ( 'NONE', #136, .T. ) ;
#7079 = AXIS2_PLACEMENT_3D ( 'NONE', #3004, #5311, #1819 ) ;
#7080 = EDGE_CURVE ( 'NONE', #6334, #4599, #6998, .T. ) ;
#7081 = VERTEX_POINT ( 'NONE', #6435 ) ;
#7082 = ORIENTED_EDGE ( 'NONE', *, *, #3800, .F. ) ;
#7083 = FACE_OUTER_BOUND ( 'NONE', #3369, .T. ) ;
#7084 = CARTESIAN_POINT ( 'NONE',  ( 4.000000000000000000, 2.309401076758515803, -0.4999999999999995559 ) ) ;
#7085 = CARTESIAN_POINT ( 'NONE',  ( -4.000000000000000000, -1.560351142792950618, -0.2242961665059814425 ) ) ;
#7086 = CYLINDRICAL_SURFACE ( 'NONE', #1607, 12.44999999999999929 ) ;
#7087 = AXIS2_PLACEMENT_3D ( 'NONE', #4272, #130, #5325 ) ;
#7088 = CARTESIAN_POINT ( 'NONE',  ( -2.682243648011671588, -3.070208061305317759, -0.04852650426602272971 ) ) ;
#7089 = LINE ( 'NONE', #1942, #7101 ) ;
#7090 = ADVANCED_BREP_SHAPE_REPRESENTATION ( '', ( #5701, #1963 ), #4003 ) ;
#7091 = ORIENTED_EDGE ( 'NONE', *, *, #6351, .T. ) ;
#7092 = PRODUCT_DEFINITION_SHAPE ( 'NONE', 'NONE',  #7348 ) ;
#7093 = ADVANCED_FACE ( 'NONE', ( #1297 ), #4746, .F. ) ;
#7094 = AXIS2_PLACEMENT_3D ( 'NONE', #2909, #6936, #3510 ) ;
#7095 = CARTESIAN_POINT ( 'NONE',  ( 2.100000000000000089, 0.000000000000000000, -4.694516984716113228 ) ) ;
#7096 = ORIENTED_EDGE ( 'NONE', *, *, #5401, .T. ) ;
#7097 = AXIS2_PLACEMENT_3D ( 'NONE', #2633, #3683, #967 ) ;
#7098 = EDGE_CURVE ( 'NONE', #1949, #431, #557, .T. ) ;
#7099 = LINE ( 'NONE', #5827, #291 ) ;
#7100 = CARTESIAN_POINT ( 'NONE',  ( 435.0000000000000568, -8.660254037844389075, 139.9990000000000236 ) ) ;
#7101 = VECTOR ( 'NONE', #3668, 1000.000000000000000 ) ;
#7102 = VERTEX_POINT ( 'NONE', #255 ) ;
#7103 = EDGE_CURVE ( 'NONE', #828, #6959, #6893, .T. ) ;
#7104 = ORIENTED_EDGE ( 'NONE', *, *, #6956, .F. ) ;
#7105 = CARTESIAN_POINT ( 'NONE',  ( 1.654252653721905331, 3.663718938583014229, -0.01223254789873410957 ) ) ;
#7106 = AXIS2_PLACEMENT_3D ( 'NONE', #1937, #1392, #2978 ) ;
#7107 = DIRECTION ( 'NONE',  ( 1.000000000000000000, 0.000000000000000000, 0.000000000000000000 ) ) ;
#7108 = CIRCLE ( 'NONE', #657, 12.77499999999999858 ) ;
#7109 = DIRECTION ( 'NONE',  ( 0.000000000000000000, 0.000000000000000000, 1.000000000000000000 ) ) ;
#7110 = VECTOR ( 'NONE', #5348, 1000.000000000000000 ) ;
#7111 = ORIENTED_EDGE ( 'NONE', *, *, #1321, .F. ) ;
#7112 = CARTESIAN_POINT ( 'NONE',  ( 445.0000000000000000, 8.660254037844390851, 140.0000000000000000 ) ) ;
#7113 = FACE_OUTER_BOUND ( 'NONE', #3838, .T. ) ;
#7114 = CIRCLE ( 'NONE', #1845, 2.649999999999985700 ) ;
#7115 = ORIENTED_EDGE ( 'NONE', *, *, #6851, .T. ) ;
#7116 = DIRECTION ( 'NONE',  ( 0.000000000000000000, 1.000000000000000000, 0.000000000000000000 ) ) ;
#7117 = ORIENTED_EDGE ( 'NONE', *, *, #3033, .F. ) ;
#7118 = VECTOR ( 'NONE', #4488, 1000.000000000000000 ) ;
#7119 = EDGE_LOOP ( 'NONE', ( #441, #2279, #2754, #4337 ) ) ;
#7120 = CARTESIAN_POINT ( 'NONE',  ( 303.3333333333333144, -15.00000000000000000, 159.8500000000001080 ) ) ;
#7121 = VECTOR ( 'NONE', #6132, 1000.000000000000000 ) ;
#7122 = CARTESIAN_POINT ( 'NONE',  ( -1.274258131565027874, -3.883108878240886241, -3.220599429844051009 ) ) ;
#7123 = CARTESIAN_POINT ( 'NONE',  ( 19.00000000000000000, 2.326828918379970970E-15, 125.0000000000000000 ) ) ;
#7124 = CARTESIAN_POINT ( 'NONE',  ( -4.000000000000000000, 0.7924765000094600165, -0.05906175389889745803 ) ) ;
#7125 = EDGE_CURVE ( 'NONE', #4282, #5338, #2326, .T. ) ;
#7126 = DIRECTION ( 'NONE',  ( 0.000000000000000000, 1.000000000000000000, -1.224646799147353207E-16 ) ) ;
#7127 = CIRCLE ( 'NONE', #6419, 2.649999999999985700 ) ;
#7128 = ORIENTED_EDGE ( 'NONE', *, *, #5834, .F. ) ;
#7129 = DIRECTION ( 'NONE',  ( -0.000000000000000000, -0.000000000000000000, -1.000000000000000000 ) ) ;
#7130 = CARTESIAN_POINT ( 'NONE',  ( 1.799999999999996048, 0.000000000000000000, 0.000000000000000000 ) ) ;
#7131 = ORIENTED_EDGE ( 'NONE', *, *, #1710, .F. ) ;
#7132 = CARTESIAN_POINT ( 'NONE',  ( -30.00000000000002842, -20.00000000000000000, -200.0000000000000000 ) ) ;
#7133 = AXIS2_PLACEMENT_3D ( 'NONE', #5229, #2474, #6433 ) ;
#7134 =( NAMED_UNIT ( * ) SI_UNIT ( $, .STERADIAN. ) SOLID_ANGLE_UNIT ( ) );
#7135 =( REPRESENTATION_RELATIONSHIP ('NONE','NONE', #5587, #6025 ) REPRESENTATION_RELATIONSHIP_WITH_TRANSFORMATION ( #6265 )SHAPE_REPRESENTATION_RELATIONSHIP( ) );
#7136 = EDGE_CURVE ( 'NONE', #6037, #1596, #3220, .T. ) ;
#7137 = DIRECTION ( 'NONE',  ( -0.000000000000000000, -0.000000000000000000, 1.000000000000000000 ) ) ;
#7138 = ORIENTED_EDGE ( 'NONE', *, *, #1690, .T. ) ;
#7139 = ORIENTED_EDGE ( 'NONE', *, *, #3712, .F. ) ;
#7140 = CARTESIAN_POINT ( 'NONE',  ( -5.000000000000000888, 8.660254037844390851, 150.0000000000000000 ) ) ;
#7141 = EDGE_CURVE ( 'NONE', #3826, #3869, #4213, .T. ) ;
#7142 = FACE_OUTER_BOUND ( 'NONE', #1890, .T. ) ;
#7143 = FACE_OUTER_BOUND ( 'NONE', #232, .T. ) ;
#7144 = VERTEX_POINT ( 'NONE', #409 ) ;
#7145 = EDGE_CURVE ( 'NONE', #3261, #1397, #3183, .T. ) ;
#7146 = FACE_OUTER_BOUND ( 'NONE', #4345, .T. ) ;
#7147 = CONTEXT_DEPENDENT_SHAPE_REPRESENTATION ( #6285, #797 ) ;
#7148 = CARTESIAN_POINT ( 'NONE',  ( 386.6666666666666288, -20.00000000000000000, 159.8500000000001080 ) ) ;
#7149 = CARTESIAN_POINT ( 'NONE',  ( 0.000000000000000000, 0.000000000000000000, 121.0000000000000000 ) ) ;
#7150 = CARTESIAN_POINT ( 'NONE',  ( 439.9999999999999432, 0.000000000000000000, 0.000000000000000000 ) ) ;
#7151 = ORIENTED_EDGE ( 'NONE', *, *, #623, .F. ) ;
#7152 = FACE_BOUND ( 'NONE', #3161, .T. ) ;
#7153 = PRODUCT ( 'hex flange nut gradea_iso_ISO - 4161 - M5 - N', 'hex flange nut gradea_iso_ISO - 4161 - M5 - N', '', ( #6173 ) ) ;
#7154 = ORIENTED_EDGE ( 'NONE', *, *, #3426, .F. ) ;
#7155 = VERTEX_POINT ( 'NONE', #367 ) ;
#7156 = DIRECTION ( 'NONE',  ( 0.000000000000000000, 0.000000000000000000, -1.000000000000000000 ) ) ;
#7157 = CARTESIAN_POINT ( 'NONE',  ( 405.0000000000000000, 8.660254037844390851, 140.0000000000000000 ) ) ;
#7158 = CARTESIAN_POINT ( 'NONE',  ( 285.0000000000000568, 8.660254037844390851, 145.0000000000000284 ) ) ;
#7159 = DIRECTION ( 'NONE',  ( 0.000000000000000000, 0.000000000000000000, -1.000000000000000000 ) ) ;
#7160 = EDGE_CURVE ( 'NONE', #5784, #630, #2631, .T. ) ;
#7161 = FACE_OUTER_BOUND ( 'NONE', #126, .T. ) ;
#7162 = CARTESIAN_POINT ( 'NONE',  ( 219.9999999999999716, -20.00000000000000000, 162.5000000000000853 ) ) ;
#7163 = EDGE_LOOP ( 'NONE', ( #689, #4838 ) ) ;
#7164 = FACE_OUTER_BOUND ( 'NONE', #6820, .T. ) ;
#7165 = CARTESIAN_POINT ( 'NONE',  ( 445.0000000000000000, 8.660254037844390851, 145.0000000000000284 ) ) ;
#7166 = ORIENTED_EDGE ( 'NONE', *, *, #395, .F. ) ;
#7167 = DIRECTION ( 'NONE',  ( 0.000000000000000000, -1.000000000000000000, 0.000000000000000000 ) ) ;
#7168 = APPLICATION_PROTOCOL_DEFINITION ( 'draft international standard', 'automotive_design', 1998, #61 ) ;
#7169 = CARTESIAN_POINT ( 'NONE',  ( 2.500000000000000000, 1.178949249685213863, -2.042000000000001148 ) ) ;
#7170 = DIRECTION ( 'NONE',  ( 1.000000000000000000, 0.000000000000000000, 0.000000000000000000 ) ) ;
#7171 = ORIENTED_EDGE ( 'NONE', *, *, #5947, .T. ) ;
#7172 = EDGE_CURVE ( 'NONE', #3083, #6247, #2512, .T. ) ;
#7173 = AXIS2_PLACEMENT_3D ( 'NONE', #784, #4113, #3571 ) ;
#7174 = DIRECTION ( 'NONE',  ( 1.000000000000000000, 0.000000000000000000, 0.000000000000000000 ) ) ;
#7175 = ORIENTED_EDGE ( 'NONE', *, *, #5857, .F. ) ;
#7176 = DIRECTION ( 'NONE',  ( -1.000000000000000000, 0.000000000000000000, 0.000000000000000000 ) ) ;
#7177 = AXIS2_PLACEMENT_3D ( 'NONE', #6563, #2571, #7156 ) ;
#7178 = CARTESIAN_POINT ( 'NONE',  ( 219.9999999999999716, -20.00000000000000000, 162.5000000000000853 ) ) ;
#7179 = DIRECTION ( 'NONE',  ( 0.000000000000000000, -1.000000000000000000, 0.000000000000000000 ) ) ;
#7180 = ORIENTED_EDGE ( 'NONE', *, *, #4537, .T. ) ;
#7181 = VECTOR ( 'NONE', #3681, 1000.000000000000000 ) ;
#7182 = EDGE_CURVE ( 'NONE', #841, #4483, #2438, .T. ) ;
#7183 = PRESENTATION_LAYER_ASSIGNMENT (  '', '', ( #6844 ) ) ;
#7184 = DIRECTION ( 'NONE',  ( 1.000000000000000000, 0.000000000000000000, 0.000000000000000000 ) ) ;
#7185 = CONTEXT_DEPENDENT_SHAPE_REPRESENTATION ( #2903, #6900 ) ;
#7186 = DIRECTION ( 'NONE',  ( 1.000000000000000000, 0.000000000000000000, 0.000000000000000000 ) ) ;
#7187 = CARTESIAN_POINT ( 'NONE',  ( 4.000000000000000000, -2.309401076758516691, -0.4999999999999995559 ) ) ;
#7188 = DIRECTION ( 'NONE',  ( -1.000000000000000000, 0.000000000000000000, 0.000000000000000000 ) ) ;
#7189 = VERTEX_POINT ( 'NONE', #4289 ) ;
#7190 = FACE_OUTER_BOUND ( 'NONE', #2763, .T. ) ;
#7191 = EDGE_LOOP ( 'NONE', ( #3797, #4628 ) ) ;
#7192 = VERTEX_POINT ( 'NONE', #4850 ) ;
#7193 = EDGE_CURVE ( 'NONE', #1563, #3012, #3029, .T. ) ;
#7194 = LINE ( 'NONE', #6595, #2621 ) ;
#7195 = PLANE ( 'NONE',  #5698 ) ;
#7196 = LINE ( 'NONE', #388, #6140 ) ;
#7197 = DIRECTION ( 'NONE',  ( 1.000000000000000000, 0.000000000000000000, 0.000000000000000000 ) ) ;
#7198 = LINE ( 'NONE', #3908, #58 ) ;
#7199 = PLANE ( 'NONE',  #4969 ) ;
#7200 = DIRECTION ( 'NONE',  ( -1.000000000000000000, -0.000000000000000000, -0.000000000000000000 ) ) ;
#7201 = ORIENTED_EDGE ( 'NONE', *, *, #4328, .T. ) ;
#7202 = CIRCLE ( 'NONE', #5524, 10.00000000000000000 ) ;
#7203 = CARTESIAN_POINT ( 'NONE',  ( 75.00000000000001421, 8.660254037844390851, 140.0000000000000000 ) ) ;
#7204 = DIRECTION ( 'NONE',  ( 0.000000000000000000, 0.000000000000000000, 1.000000000000000000 ) ) ;
#7205 = ORIENTED_EDGE ( 'NONE', *, *, #4946, .T. ) ;
#7206 = FILL_AREA_STYLE_COLOUR ( '', #2626 ) ;
#7207 = CARTESIAN_POINT ( 'NONE',  ( 0.000000000000000000, 0.000000000000000000, 0.000000000000000000 ) ) ;
#7208 = PLANE ( 'NONE',  #4388 ) ;
#7209 = VECTOR ( 'NONE', #1593, 1000.000000000000000 ) ;
#7210 = ORIENTED_EDGE ( 'NONE', *, *, #7060, .F. ) ;
#7211 = CARTESIAN_POINT ( 'NONE',  ( 320.0000000000000000, 0.000000000000000000, 0.000000000000000000 ) ) ;
#7212 = EDGE_LOOP ( 'NONE', ( #1918, #2746, #6594, #2590 ) ) ;
#7213 = PRODUCT_DEFINITION_SHAPE ( 'NONE', 'NONE',  #7356 ) ;
#7214 = LINE ( 'NONE', #4254, #4975 ) ;
#7215 = AXIS2_PLACEMENT_3D ( 'NONE', #852, #7188, #6675 ) ;
#7216 = EDGE_CURVE ( 'NONE', #3032, #2165, #7214, .T. ) ;
#7217 = AXIS2_PLACEMENT_3D ( 'NONE', #3747, #6494, #6457 ) ;
#7218 = CIRCLE ( 'NONE', #5414, 13.50000000000000178 ) ;
#7219 = CARTESIAN_POINT ( 'NONE',  ( 303.3333333333333144, -20.00000000000000000, 162.5000000000000853 ) ) ;
#7220 = CARTESIAN_POINT ( 'NONE',  ( 2.500000000000000000, 1.178949249685213863, -2.042000000000001148 ) ) ;
#7221 = VERTEX_POINT ( 'NONE', #1528 ) ;
#7222 = AXIS2_PLACEMENT_3D ( 'NONE', #5124, #665, #562 ) ;
#7223 = VECTOR ( 'NONE', #3910, 1000.000000000000000 ) ;
#7224 = CARTESIAN_POINT ( 'NONE',  ( 4.000000000000000000, 1.680228229147133767, -3.316631783032546021 ) ) ;
#7225 = DIRECTION ( 'NONE',  ( 0.000000000000000000, 0.000000000000000000, -1.000000000000000000 ) ) ;
#7226 = FACE_OUTER_BOUND ( 'NONE', #5262, .T. ) ;
#7227 = CARTESIAN_POINT ( 'NONE',  ( 219.9999999999999716, -10.00000000000000000, 162.5000000000000853 ) ) ;
#7228 = ORIENTED_EDGE ( 'NONE', *, *, #3702, .T. ) ;
#7229 = VECTOR ( 'NONE', #3479, 1000.000000000000000 ) ;
#7230 = PLANE ( 'NONE',  #1462 ) ;
#7231 = ADVANCED_FACE ( 'NONE', ( #4887 ), #2029, .T. ) ;
#7232 = ADVANCED_FACE ( 'NONE', ( #6577 ), #1442, .F. ) ;
#7233 = VERTEX_POINT ( 'NONE', #5949 ) ;
#7234 = VERTEX_POINT ( 'NONE', #6069 ) ;
#7235 = CARTESIAN_POINT ( 'NONE',  ( 405.0000000000000000, 8.660254037844390851, 145.0000000000000284 ) ) ;
#7236 = CARTESIAN_POINT ( 'NONE',  ( 0.5636800770130377947, 4.293361309317166530, -3.531542292954102713 ) ) ;
#7237 = VECTOR ( 'NONE', #4116, 1000.000000000000000 ) ;
#7238 = CONTEXT_DEPENDENT_SHAPE_REPRESENTATION ( #249, #5406 ) ;
#7239 = DIRECTION ( 'NONE',  ( -1.000000000000000000, 0.000000000000000000, 0.000000000000000000 ) ) ;
#7240 = CARTESIAN_POINT ( 'NONE',  ( -4.000000000000000000, 1.941961291383472732, -0.3515519931180205448 ) ) ;
#7241 = VECTOR ( 'NONE', #867, 1000.000000000000000 ) ;
#7242 = CARTESIAN_POINT ( 'NONE',  ( -1.999999999999998224, 0.000000000000000000, 0.000000000000000000 ) ) ;
#7243 = DIRECTION ( 'NONE',  ( 0.000000000000000000, 0.000000000000000000, 1.000000000000000000 ) ) ;
#7244 = EDGE_CURVE ( 'NONE', #3697, #4862, #814, .T. ) ;
#7245 = VECTOR ( 'NONE', #2929, 1000.000000000000000 ) ;
#7246 = ORIENTED_EDGE ( 'NONE', *, *, #2101, .T. ) ;
#7247 = VECTOR ( 'NONE', #954, 1000.000000000000000 ) ;
#7248 = FACE_OUTER_BOUND ( 'NONE', #2074, .T. ) ;
#7249 = EDGE_CURVE ( 'NONE', #1000, #4634, #2083, .T. ) ;
#7250 = DIRECTION ( 'NONE',  ( 0.000000000000000000, 0.000000000000000000, 1.000000000000000000 ) ) ;
#7251 = CARTESIAN_POINT ( 'NONE',  ( 219.9999999999999716, -25.00000000000000000, 162.5000000000000853 ) ) ;
#7252 = SURFACE_STYLE_USAGE ( .BOTH. , #2064 ) ;
#7253 =( LENGTH_UNIT ( ) NAMED_UNIT ( * ) SI_UNIT ( .MILLI., .METRE. ) );
#7254 = VECTOR ( 'NONE', #88, 1000.000000000000000 ) ;
#7255 = DIRECTION ( 'NONE',  ( 0.000000000000000000, 0.000000000000000000, -1.000000000000000000 ) ) ;
#7256 = CARTESIAN_POINT ( 'NONE',  ( 355.0000000000000000, 8.660254037844390851, 145.0000000000000284 ) ) ;
#7257 = ORIENTED_EDGE ( 'NONE', *, *, #4846, .F. ) ;
#7258 = VERTEX_POINT ( 'NONE', #6022 ) ;
#7260 = CIRCLE ( 'NONE', #4256, 2.649999999999985700 ) ;
#7259 = DIRECTION ( 'NONE',  ( 6.123233995736766036E-17, -1.000000000000000000, 0.000000000000000000 ) ) ;
#7261 = ORIENTED_EDGE ( 'NONE', *, *, #4122, .F. ) ;
#7262 = DIRECTION ( 'NONE',  ( 0.000000000000000000, 0.000000000000000000, -1.000000000000000000 ) ) ;
#7263 = ADVANCED_FACE ( 'NONE', ( #3100 ), #888, .F. ) ;
#7264 = CARTESIAN_POINT ( 'NONE',  ( 303.3333333333333144, -20.00000000000000000, -162.5000000000000853 ) ) ;
#7265 = LINE ( 'NONE', #4415, #4382 ) ;
#7266 = EDGE_LOOP ( 'NONE', ( #6387, #364, #560, #48, #5332 ) ) ;
#7267 = DIRECTION ( 'NONE',  ( 1.000000000000000000, 0.000000000000000000, 0.000000000000000000 ) ) ;
#7268 = DIRECTION ( 'NONE',  ( 1.000000000000000000, 0.000000000000000000, 0.000000000000000000 ) ) ;
#7269 = DIRECTION ( 'NONE',  ( 0.000000000000000000, 0.000000000000000000, 1.000000000000000000 ) ) ;
#7270 = DIRECTION ( 'NONE',  ( 0.000000000000000000, 0.000000000000000000, 1.000000000000000000 ) ) ;
#7271 = ORIENTED_EDGE ( 'NONE', *, *, #1885, .T. ) ;
#7272 = CARTESIAN_POINT ( 'NONE',  ( -6.259644161404860030E-16, -4.618802153517027165, -3.433295621305388234 ) ) ;
#7273 = ORIENTED_EDGE ( 'NONE', *, *, #416, .F. ) ;
#7274 = EDGE_CURVE ( 'NONE', #3198, #3944, #2823, .T. ) ;
#7275 = ORIENTED_EDGE ( 'NONE', *, *, #2840, .F. ) ;
#7276 = LINE ( 'NONE', #944, #4315 ) ;
#7277 = LINE ( 'NONE', #3361, #1746 ) ;
#7278 = DIRECTION ( 'NONE',  ( -0.000000000000000000, -0.000000000000000000, -1.000000000000000000 ) ) ;
#7279 = CARTESIAN_POINT ( 'NONE',  ( -30.00000000000002842, -25.00000000000000000, -200.0000000000000000 ) ) ;
#7280 = EDGE_CURVE ( 'NONE', #1523, #5003, #596, .T. ) ;
#7281 = DIRECTION ( 'NONE',  ( -0.000000000000000000, -1.000000000000000000, -0.000000000000000000 ) ) ;
#7282 = PRODUCT_DEFINITION_CONTEXT ( 'detailed design', #678, 'design' ) ;
#7283 = DIRECTION ( 'NONE',  ( -1.000000000000000000, -0.000000000000000000, -0.000000000000000000 ) ) ;
#7284 =( REPRESENTATION_RELATIONSHIP ('NONE','NONE', #5587, #1193 ) REPRESENTATION_RELATIONSHIP_WITH_TRANSFORMATION ( #5659 )SHAPE_REPRESENTATION_RELATIONSHIP( ) );
#7285 = ORIENTED_EDGE ( 'NONE', *, *, #5435, .T. ) ;
#7286 = DIRECTION ( 'NONE',  ( -0.000000000000000000, -0.000000000000000000, -1.000000000000000000 ) ) ;
#7287 = DIRECTION ( 'NONE',  ( 1.000000000000000000, 0.000000000000000000, 0.000000000000000000 ) ) ;
#7288 = CARTESIAN_POINT ( 'NONE',  ( 1.828356344711641102, 3.563200125723180900, -5.433716356636336675E-16 ) ) ;
#7289 = SURFACE_STYLE_FILL_AREA ( #3756 ) ;
#7290 = EDGE_CURVE ( 'NONE', #6714, #7155, #3425, .T. ) ;
#7291 =( NAMED_UNIT ( * ) PLANE_ANGLE_UNIT ( ) SI_UNIT ( $, .RADIAN. ) );
#7292 = FACE_OUTER_BOUND ( 'NONE', #4925, .T. ) ;
#7293 = VERTEX_POINT ( 'NONE', #491 ) ;
#7294 = VERTEX_POINT ( 'NONE', #6739 ) ;
#7295 = DIRECTION ( 'NONE',  ( 0.000000000000000000, 0.000000000000000000, -1.000000000000000000 ) ) ;
#7296 = ORIENTED_EDGE ( 'NONE', *, *, #3973, .F. ) ;
#7297 = EDGE_CURVE ( 'NONE', #6176, #3944, #2851, .T. ) ;
#7298 = CARTESIAN_POINT ( 'NONE',  ( 2.500000000000000000, 1.178949249685213863, -2.042000000000001148 ) ) ;
#7299 = CARTESIAN_POINT ( 'NONE',  ( -2.500000000000000444, 3.061616997868383634E-16, -5.000000000000000888 ) ) ;
#7300 = DIRECTION ( 'NONE',  ( 1.000000000000000000, 0.000000000000000000, 0.000000000000000000 ) ) ;
#7301 = ORIENTED_EDGE ( 'NONE', *, *, #1641, .F. ) ;
#7302 = PRODUCT_RELATED_PRODUCT_CATEGORY ( 'part', '', ( #870 ) ) ;
#7303 = DIRECTION ( 'NONE',  ( 0.000000000000000000, -0.000000000000000000, -1.000000000000000000 ) ) ;
#7304 = CARTESIAN_POINT ( 'NONE',  ( 0.000000000000000000, 0.000000000000000000, 0.000000000000000000 ) ) ;
#7305 = DIRECTION ( 'NONE',  ( -0.000000000000000000, 1.000000000000000000, -0.000000000000000000 ) ) ;
#7306 = DIRECTION ( 'NONE',  ( -1.000000000000000000, 0.000000000000000000, 0.000000000000000000 ) ) ;
#7307 = VERTEX_POINT ( 'NONE', #5126 ) ;
#7308 = VERTEX_POINT ( 'NONE', #6181 ) ;
#7309 = VERTEX_POINT ( 'NONE', #566 ) ;
#7310 = CARTESIAN_POINT ( 'NONE',  ( 4.999999999999999112, -8.660254037844389075, 150.0000000000000000 ) ) ;
#7311 = DIRECTION ( 'NONE',  ( -0.000000000000000000, -1.000000000000000000, -0.000000000000000000 ) ) ;
#7312 = CONTEXT_DEPENDENT_SHAPE_REPRESENTATION ( #4691, #6970 ) ;
#7313 = CARTESIAN_POINT ( 'NONE',  ( 0.000000000000000000, 0.000000000000000000, 140.0000000000000000 ) ) ;
#7314 = PLANE ( 'NONE',  #5194 ) ;
#7315 = VECTOR ( 'NONE', #955, 1000.000000000000000 ) ;
#7316 = VECTOR ( 'NONE', #6126, 1000.000000000000000 ) ;
#7317 = B_SPLINE_CURVE_WITH_KNOTS ( 'NONE', 3,
 ( #2952, #144, #182, #2364, #2398 ),
 .UNSPECIFIED., .F., .F.,
 ( 4, 1, 4 ),
 ( 0.000000000000000000, 0.002309401076758505356, 0.004618802153517010713 ),
 .UNSPECIFIED. ) ;
#7318 = CARTESIAN_POINT ( 'NONE',  ( 1.800000000000001155, 0.000000000000000000, 0.000000000000000000 ) ) ;
#7319 = CARTESIAN_POINT ( 'NONE',  ( 53.33333333333330017, -25.00000000000000000, -162.5000000000000853 ) ) ;
#7320 = EDGE_CURVE ( 'NONE', #2711, #5499, #6781, .T. ) ;
#7321 = EDGE_LOOP ( 'NONE', ( #663, #1659, #4323, #5702 ) ) ;
#7322 = FACE_OUTER_BOUND ( 'NONE', #4416, .T. ) ;
#7323 = FACE_OUTER_BOUND ( 'NONE', #6854, .T. ) ;
#7324 = B_SPLINE_CURVE_WITH_KNOTS ( 'NONE', 3,
 ( #2722, #5021, #4453, #2177, #6544, #7105, #7288, #6692 ),
 .UNSPECIFIED., .F., .F.,
 ( 4, 2, 2, 4 ),
 ( 2.465131517075058656E-07, 0.001183067374689851080, 0.001774477805458923299, 0.002365888236227995517 ),
 .UNSPECIFIED. ) ;
#7325 = DIRECTION ( 'NONE',  ( 0.000000000000000000, 1.000000000000000000, 0.000000000000000000 ) ) ;
#7326 = DIRECTION ( 'NONE',  ( 1.000000000000000000, 0.000000000000000000, 0.000000000000000000 ) ) ;
#7327 = PRESENTATION_STYLE_ASSIGNMENT (( #5772 ) ) ;
#7328 = DIRECTION ( 'NONE',  ( 1.000000000000000000, 0.000000000000000000, 0.000000000000000000 ) ) ;
#7329 = APPLICATION_CONTEXT ( 'automotive_design' ) ;
#7330 = ADVANCED_FACE ( 'NONE', ( #3346 ), #5688, .F. ) ;
#7331 = ORIENTED_EDGE ( 'NONE', *, *, #6321, .F. ) ;
#7332 = VERTEX_POINT ( 'NONE', #2153 ) ;
#7333 = TOROIDAL_SURFACE ( 'NONE', #6328, 2.700000000000001066, 0.2000000000000000111 ) ;
#7334 = CARTESIAN_POINT ( 'NONE',  ( 240.0000000000000000, 0.000000000000000000, 0.000000000000000000 ) ) ;
#7335 = EDGE_LOOP ( 'NONE', ( #2395, #408, #700, #4515 ) ) ;
#7336 = DIRECTION ( 'NONE',  ( 0.000000000000000000, -1.000000000000000000, 0.000000000000000000 ) ) ;
#7337 = COLOUR_RGB ( '',0.8941176470588234615, 0.8941176470588234615, 0.8941176470588234615 ) ;
#7338 = DIRECTION ( 'NONE',  ( 0.000000000000000000, 0.000000000000000000, 1.000000000000000000 ) ) ;
#7339 = ADVANCED_FACE ( 'NONE', ( #5571 ), #4446, .F. ) ;
#7340 = VERTEX_POINT ( 'NONE', #3266 ) ;
#7341 = NEXT_ASSEMBLY_USAGE_OCCURRENCE ( 'NAUO1', ' ', ' ', #4274, #6666, $ ) ;
#7342 = NEXT_ASSEMBLY_USAGE_OCCURRENCE ( 'NAUO2', ' ', ' ', #4274, #3195, $ ) ;
#7343 = NEXT_ASSEMBLY_USAGE_OCCURRENCE ( 'NAUO3', ' ', ' ', #4274, #2657, $ ) ;
#7344 = NEXT_ASSEMBLY_USAGE_OCCURRENCE ( 'NAUO4', ' ', ' ', #4274, #1667, $ ) ;
#7345 = NEXT_ASSEMBLY_USAGE_OCCURRENCE ( 'NAUO5', ' ', ' ', #4274, #6385, $ ) ;
#7346 = NEXT_ASSEMBLY_USAGE_OCCURRENCE ( 'NAUO6', ' ', ' ', #4274, #6385, $ ) ;
#7347 = NEXT_ASSEMBLY_USAGE_OCCURRENCE ( 'NAUO7', ' ', ' ', #4274, #3304, $ ) ;
#7348 = NEXT_ASSEMBLY_USAGE_OCCURRENCE ( 'NAUO8', ' ', ' ', #4274, #3304, $ ) ;
#7349 = NEXT_ASSEMBLY_USAGE_OCCURRENCE ( 'NAUO9', ' ', ' ', #4274, #3304, $ ) ;
#7350 = NEXT_ASSEMBLY_USAGE_OCCURRENCE ( 'NAUO10', ' ', ' ', #4274, #3304, $ ) ;
#7351 = NEXT_ASSEMBLY_USAGE_OCCURRENCE ( 'NAUO11', ' ', ' ', #4274, #3304, $ ) ;
#7352 = NEXT_ASSEMBLY_USAGE_OCCURRENCE ( 'NAUO12', ' ', ' ', #4274, #213, $ ) ;
#7353 = NEXT_ASSEMBLY_USAGE_OCCURRENCE ( 'NAUO13', ' ', ' ', #4274, #213, $ ) ;
#7354 = NEXT_ASSEMBLY_USAGE_OCCURRENCE ( 'NAUO14', ' ', ' ', #4274, #213, $ ) ;
#7355 = NEXT_ASSEMBLY_USAGE_OCCURRENCE ( 'NAUO15', ' ', ' ', #4274, #213, $ ) ;
#7356 = NEXT_ASSEMBLY_USAGE_OCCURRENCE ( 'NAUO16', ' ', ' ', #4274, #213, $ ) ;
#7357 = NEXT_ASSEMBLY_USAGE_OCCURRENCE ( 'NAUO17', ' ', ' ', #4274, #2657, $ ) ;
#7358 = NEXT_ASSEMBLY_USAGE_OCCURRENCE ( 'NAUO18', ' ', ' ', #4274, #6385, $ ) ;
#7359 = NEXT_ASSEMBLY_USAGE_OCCURRENCE ( 'NAUO19', ' ', ' ', #4274, #6385, $ ) ;
#7360 = NEXT_ASSEMBLY_USAGE_OCCURRENCE ( 'NAUO20', ' ', ' ', #4274, #6385, $ ) ;
#7361 = NEXT_ASSEMBLY_USAGE_OCCURRENCE ( 'NAUO21', ' ', ' ', #4274, #6385, $ ) ;
#7362 = NEXT_ASSEMBLY_USAGE_OCCURRENCE ( 'NAUO22', ' ', ' ', #4274, #6385, $ ) ;
#7363 = NEXT_ASSEMBLY_USAGE_OCCURRENCE ( 'NAUO23', ' ', ' ', #4274, #6666, $ ) ;
#7364 = NEXT_ASSEMBLY_USAGE_OCCURRENCE ( 'NAUO24', ' ', ' ', #4274, #6666, $ ) ;
#7365 = NEXT_ASSEMBLY_USAGE_OCCURRENCE ( 'NAUO25', ' ', ' ', #4274, #6666, $ ) ;
#7366 = NEXT_ASSEMBLY_USAGE_OCCURRENCE ( 'NAUO26', ' ', ' ', #4274, #6666, $ ) ;
#7367 = NEXT_ASSEMBLY_USAGE_OCCURRENCE ( 'NAUO27', ' ', ' ', #4274, #6666, $ ) ;
#7368 = NEXT_ASSEMBLY_USAGE_OCCURRENCE ( 'NAUO28', ' ', ' ', #4274, #6385, $ ) ;
#7369 = NEXT_ASSEMBLY_USAGE_OCCURRENCE ( 'NAUO29', ' ', ' ', #4274, #6385, $ ) ;
#7370 = NEXT_ASSEMBLY_USAGE_OCCURRENCE ( 'NAUO30', ' ', ' ', #4274, #6385, $ ) ;
#7371 = NEXT_ASSEMBLY_USAGE_OCCURRENCE ( 'NAUO31', ' ', ' ', #4274, #6385, $ ) ;
#7372 = NEXT_ASSEMBLY_USAGE_OCCURRENCE ( 'NAUO32', ' ', ' ', #4274, #6385, $ ) ;
#7373 = NEXT_ASSEMBLY_USAGE_OCCURRENCE ( 'NAUO33', ' ', ' ', #4274, #3195, $ ) ;
#7374 = NEXT_ASSEMBLY_USAGE_OCCURRENCE ( 'NAUO34', ' ', ' ', #4274, #3195, $ ) ;
#7375 = NEXT_ASSEMBLY_USAGE_OCCURRENCE ( 'NAUO35', ' ', ' ', #4274, #3195, $ ) ;
#7376 = NEXT_ASSEMBLY_USAGE_OCCURRENCE ( 'NAUO36', ' ', ' ', #4274, #3195, $ ) ;
#7377 = NEXT_ASSEMBLY_USAGE_OCCURRENCE ( 'NAUO37', ' ', ' ', #4274, #3195, $ ) ;
#7378 = NEXT_ASSEMBLY_USAGE_OCCURRENCE ( 'NAUO38', ' ', ' ', #4274, #213, $ ) ;
#7379 = NEXT_ASSEMBLY_USAGE_OCCURRENCE ( 'NAUO39', ' ', ' ', #4274, #213, $ ) ;
#7380 = NEXT_ASSEMBLY_USAGE_OCCURRENCE ( 'NAUO40', ' ', ' ', #4274, #3304, $ ) ;
#7381 = NEXT_ASSEMBLY_USAGE_OCCURRENCE ( 'NAUO41', ' ', ' ', #4274, #213, $ ) ;
#7382 = NEXT_ASSEMBLY_USAGE_OCCURRENCE ( 'NAUO42', ' ', ' ', #4274, #3304, $ ) ;
#7383 = NEXT_ASSEMBLY_USAGE_OCCURRENCE ( 'NAUO43', ' ', ' ', #4274, #3304, $ ) ;
#7384 = NEXT_ASSEMBLY_USAGE_OCCURRENCE ( 'NAUO44', ' ', ' ', #4274, #3304, $ ) ;
#7385 = NEXT_ASSEMBLY_USAGE_OCCURRENCE ( 'NAUO45', ' ', ' ', #4274, #3304, $ ) ;
#7386 = NEXT_ASSEMBLY_USAGE_OCCURRENCE ( 'NAUO46', ' ', ' ', #4274, #213, $ ) ;
#7387 = NEXT_ASSEMBLY_USAGE_OCCURRENCE ( 'NAUO47', ' ', ' ', #4274, #213, $ ) ;
#7388 = NEXT_ASSEMBLY_USAGE_OCCURRENCE ( 'NAUO48', ' ', ' ', #4274, #3195, $ ) ;
#7389 = NEXT_ASSEMBLY_USAGE_OCCURRENCE ( 'NAUO49', ' ', ' ', #4274, #3195, $ ) ;
#7390 = NEXT_ASSEMBLY_USAGE_OCCURRENCE ( 'NAUO50', ' ', ' ', #4274, #3195, $ ) ;
#7391 = NEXT_ASSEMBLY_USAGE_OCCURRENCE ( 'NAUO51', ' ', ' ', #4274, #3195, $ ) ;
#7392 = NEXT_ASSEMBLY_USAGE_OCCURRENCE ( 'NAUO52', ' ', ' ', #4274, #3195, $ ) ;
#7393 = NEXT_ASSEMBLY_USAGE_OCCURRENCE ( 'NAUO53', ' ', ' ', #4274, #3195, $ ) ;
#7394 = NEXT_ASSEMBLY_USAGE_OCCURRENCE ( 'NAUO54', ' ', ' ', #4274, #6385, $ ) ;
#7395 = NEXT_ASSEMBLY_USAGE_OCCURRENCE ( 'NAUO55', ' ', ' ', #4274, #6385, $ ) ;
#7396 = NEXT_ASSEMBLY_USAGE_OCCURRENCE ( 'NAUO56', ' ', ' ', #4274, #6385, $ ) ;
#7397 = NEXT_ASSEMBLY_USAGE_OCCURRENCE ( 'NAUO57', ' ', ' ', #4274, #6385, $ ) ;
#7398 = NEXT_ASSEMBLY_USAGE_OCCURRENCE ( 'NAUO58', ' ', ' ', #4274, #6385, $ ) ;
#7399 = NEXT_ASSEMBLY_USAGE_OCCURRENCE ( 'NAUO59', ' ', ' ', #4274, #6385, $ ) ;
#7400 = NEXT_ASSEMBLY_USAGE_OCCURRENCE ( 'NAUO60', ' ', ' ', #4274, #6666, $ ) ;
#7401 = NEXT_ASSEMBLY_USAGE_OCCURRENCE ( 'NAUO61', ' ', ' ', #4274, #6666, $ ) ;
#7402 = NEXT_ASSEMBLY_USAGE_OCCURRENCE ( 'NAUO62', ' ', ' ', #4274, #6666, $ ) ;
#7403 = NEXT_ASSEMBLY_USAGE_OCCURRENCE ( 'NAUO63', ' ', ' ', #4274, #6666, $ ) ;
#7404 = NEXT_ASSEMBLY_USAGE_OCCURRENCE ( 'NAUO64', ' ', ' ', #4274, #6666, $ ) ;
#7405 = NEXT_ASSEMBLY_USAGE_OCCURRENCE ( 'NAUO65', ' ', ' ', #4274, #6666, $ ) ;
#7406 = NEXT_ASSEMBLY_USAGE_OCCURRENCE ( 'NAUO66', ' ', ' ', #4274, #6385, $ ) ;
#7407 = NEXT_ASSEMBLY_USAGE_OCCURRENCE ( 'NAUO67', ' ', ' ', #4274, #6385, $ ) ;
#7408 = NEXT_ASSEMBLY_USAGE_OCCURRENCE ( 'NAUO68', ' ', ' ', #4274, #6385, $ ) ;
#7409 = NEXT_ASSEMBLY_USAGE_OCCURRENCE ( 'NAUO69', ' ', ' ', #4274, #6385, $ ) ;
#7410 = NEXT_ASSEMBLY_USAGE_OCCURRENCE ( 'NAUO70', ' ', ' ', #4274, #6385, $ ) ;
#7411 = NEXT_ASSEMBLY_USAGE_OCCURRENCE ( 'NAUO71', ' ', ' ', #4274, #6385, $ ) ;
#7412=COLOUR_RGB('Dark Blue',0.08,0.2,0.34);
#7413=FILL_AREA_STYLE_COLOUR('',#7412);
#7414=FILL_AREA_STYLE('',(#7413));
#7415=SURFACE_STYLE_FILL_AREA(#7414);
#7416=SURFACE_SIDE_STYLE('',(#7415));
#7417=SURFACE_STYLE_USAGE(.BOTH.,#7416);
#7418=PRESENTATION_STYLE_ASSIGNMENT((#7417));
#7419=COLOUR_RGB('Light Blue',0.38,0.62,0.78);
#7420=FILL_AREA_STYLE_COLOUR('',#7419);
#7421=FILL_AREA_STYLE('',(#7420));
#7422=SURFACE_STYLE_FILL_AREA(#7421);
#7423=SURFACE_SIDE_STYLE('',(#7422));
#7424=SURFACE_STYLE_USAGE(.BOTH.,#7423);
#7425=PRESENTATION_STYLE_ASSIGNMENT((#7424));
#7426=COLOUR_RGB('Sky Blue',0.24,0.69,0.87);
#7427=FILL_AREA_STYLE_COLOUR('',#7426);
#7428=FILL_AREA_STYLE('',(#7427));
#7429=SURFACE_STYLE_FILL_AREA(#7428);
#7430=SURFACE_SIDE_STYLE('',(#7429));
#7431=SURFACE_STYLE_USAGE(.BOTH.,#7430);
#7432=PRESENTATION_STYLE_ASSIGNMENT((#7431));
#7433=COLOUR_RGB('Grey',0.48,0.52,0.57);
#7434=FILL_AREA_STYLE_COLOUR('',#7433);
#7435=FILL_AREA_STYLE('',(#7434));
#7436=SURFACE_STYLE_FILL_AREA(#7435);
#7437=SURFACE_SIDE_STYLE('',(#7436));
#7438=SURFACE_STYLE_USAGE(.BOTH.,#7437);
#7439=PRESENTATION_STYLE_ASSIGNMENT((#7438));
#7440=COLOUR_RGB('Black',0.12,0.14,0.17);
#7441=FILL_AREA_STYLE_COLOUR('',#7440);
#7442=FILL_AREA_STYLE('',(#7441));
#7443=SURFACE_STYLE_FILL_AREA(#7442);
#7444=SURFACE_SIDE_STYLE('',(#7443));
#7445=SURFACE_STYLE_USAGE(.BOTH.,#7444);
#7446=PRESENTATION_STYLE_ASSIGNMENT((#7445));
#7447=COLOUR_RGB('Off White',0.89,0.88,0.83);
#7448=FILL_AREA_STYLE_COLOUR('',#7447);
#7449=FILL_AREA_STYLE('',(#7448));
#7450=SURFACE_STYLE_FILL_AREA(#7449);
#7451=SURFACE_SIDE_STYLE('',(#7450));
#7452=SURFACE_STYLE_USAGE(.BOTH.,#7451);
#7453=PRESENTATION_STYLE_ASSIGNMENT((#7452));
ENDSEC;
END-ISO-10303-21;
